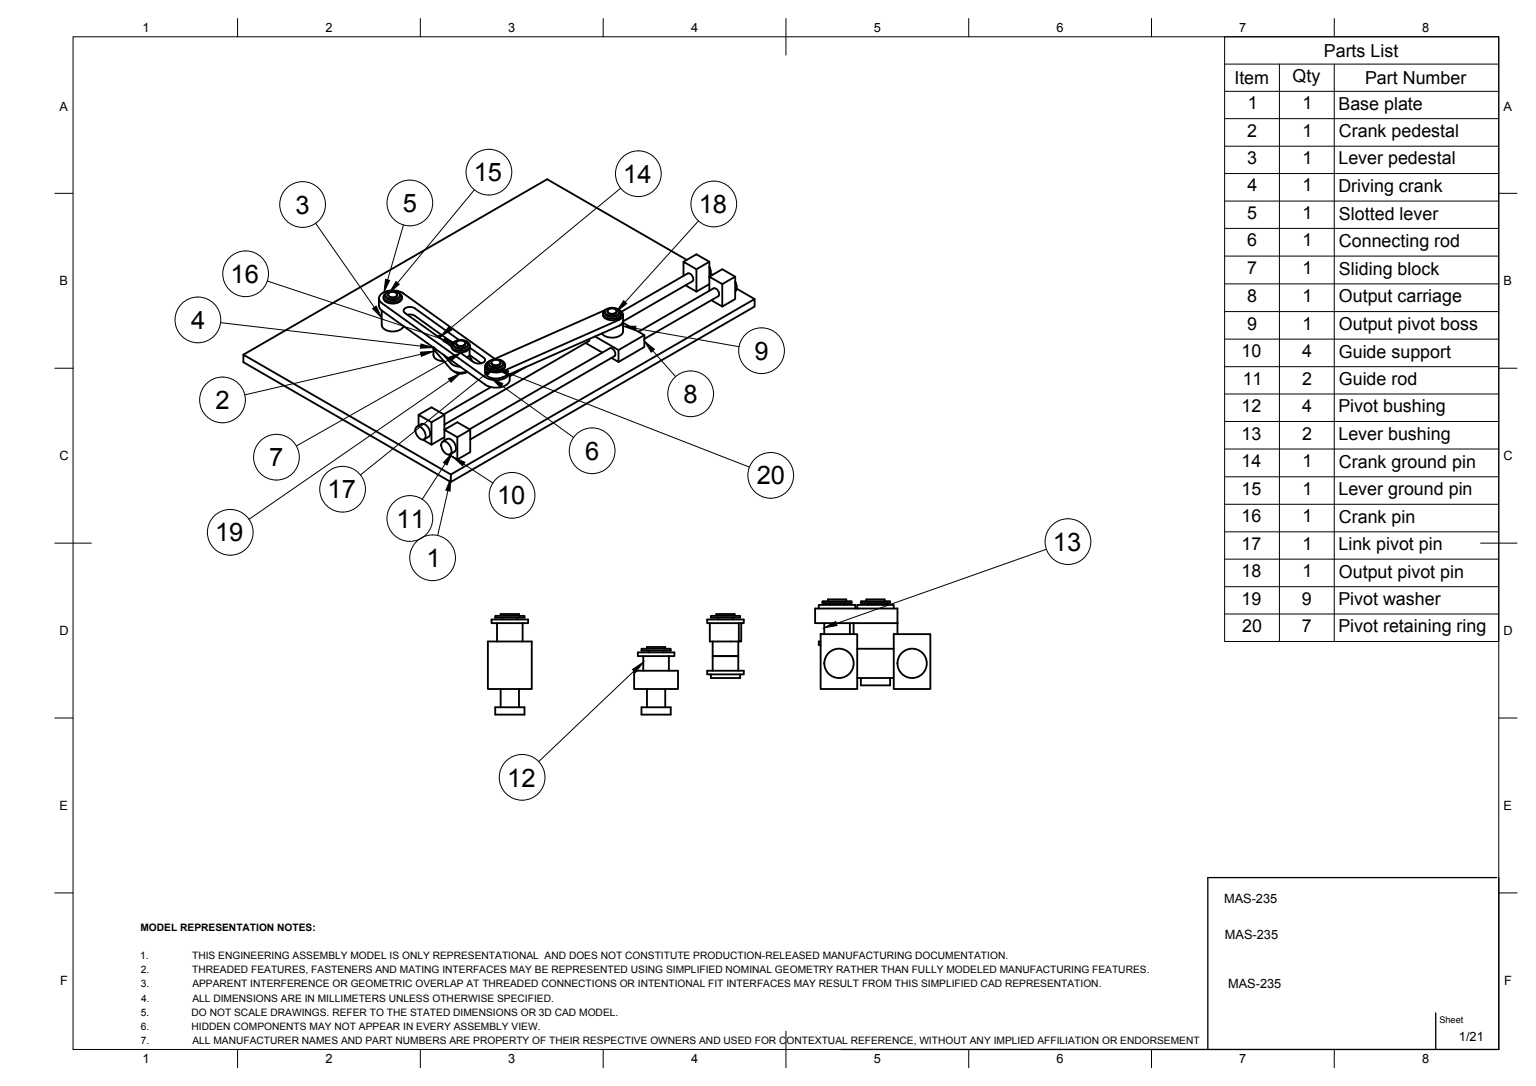
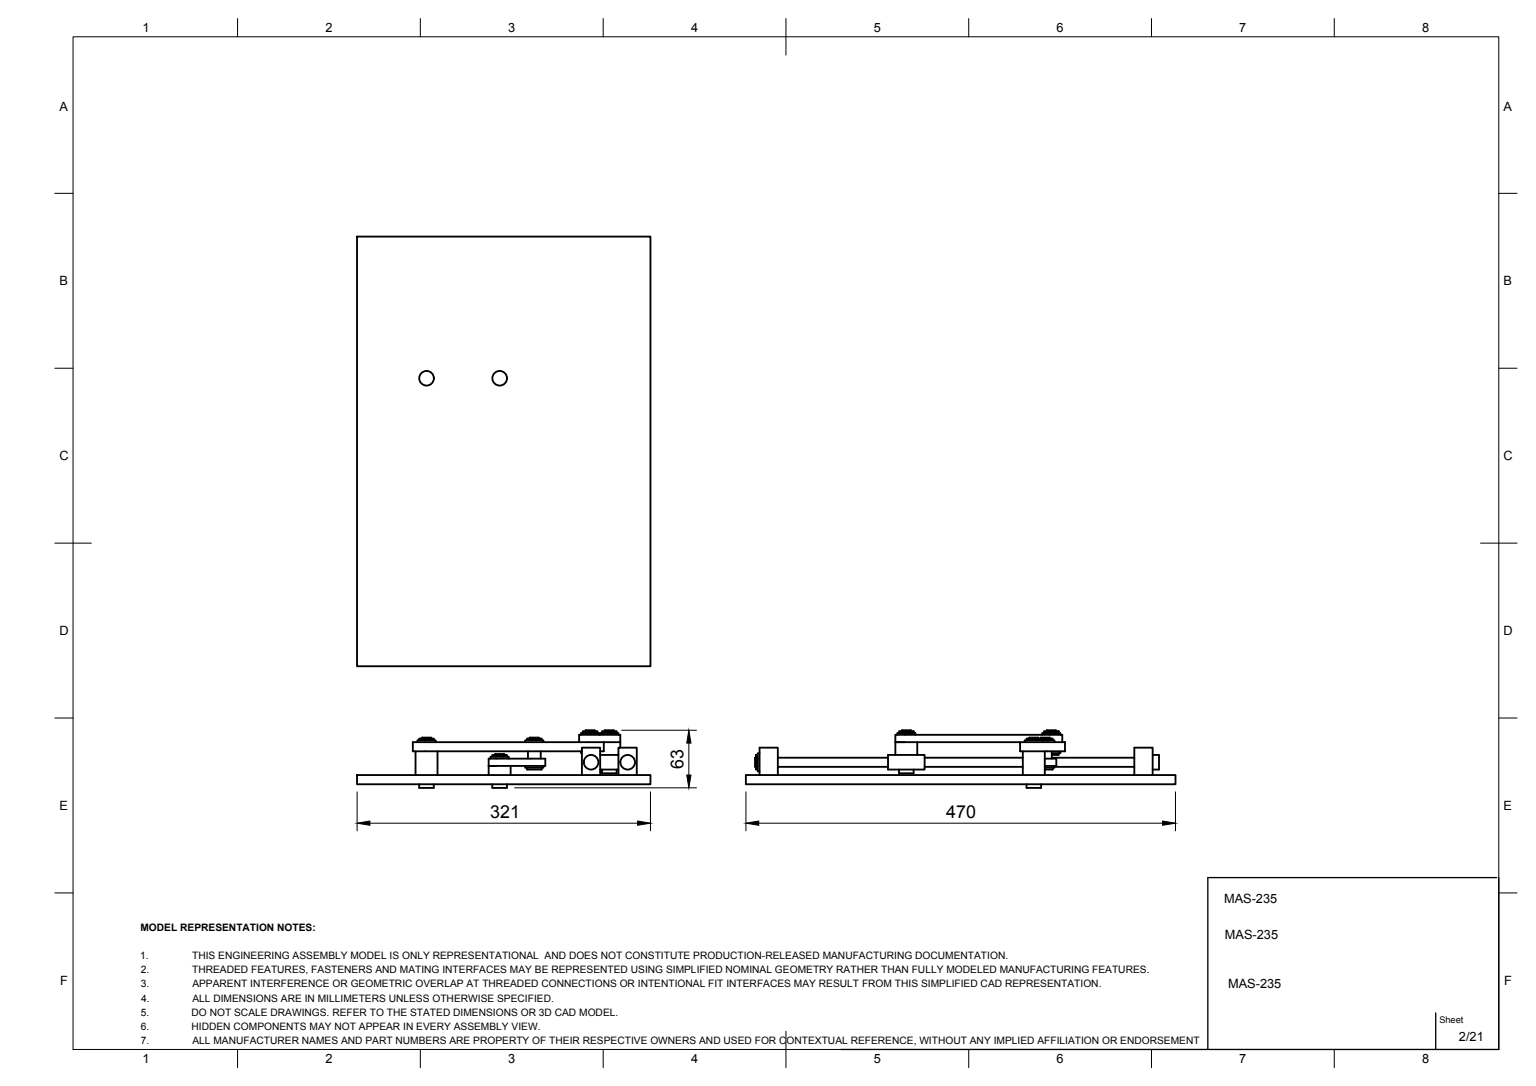
ISO-10303-21;
HEADER;
/* Generated by software containing ST-Developer
 * from STEP Tools, Inc. (www.steptools.com) 
 */

FILE_DESCRIPTION(
/* description */ ('Independent Whitworth quick-return mechanism. Crank radius40, ground-
center spacing80, lever180, connecting rod160, output guide X200. Nomi
nal stroke180 and long/short phase ratio2. Retained guide rods, replac
eable bearing sleeves and captured sliding shoe. No load or production
 rating assigned.'),
/* implementation_level */ '2;1');

FILE_NAME(
/* name */ 'MAS-235.step',
/* time_stamp */ '2026-11-09T18:22:56-08:00',
/* author */ (''),
/* organization */ (''),
/* preprocessor_version */ 'ST-DEVELOPER v20.2',
/* originating_system */ 'Autodesk Translation Framework v15.17.0.0',
/* authorisation */ '');

FILE_SCHEMA (('AUTOMOTIVE_DESIGN { 1 0 10303 214 3 1 1 }'));
ENDSEC;

DATA;
#10=MECHANICAL_DESIGN_GEOMETRIC_PRESENTATION_REPRESENTATION('',(#219,#220,
#221,#222,#223,#224,#225,#226,#227,#228,#229,#230,#231,#232,#233,#234,#235,
#236,#237,#238),#4388);
#11=ITEM_DEFINED_TRANSFORMATION($,$,#2566,#2855);
#12=ITEM_DEFINED_TRANSFORMATION($,$,#2579,#2856);
#13=ITEM_DEFINED_TRANSFORMATION($,$,#2588,#2857);
#14=ITEM_DEFINED_TRANSFORMATION($,$,#2597,#2858);
#15=ITEM_DEFINED_TRANSFORMATION($,$,#2614,#2859);
#16=ITEM_DEFINED_TRANSFORMATION($,$,#2639,#2860);
#17=ITEM_DEFINED_TRANSFORMATION($,$,#2656,#2861);
#18=ITEM_DEFINED_TRANSFORMATION($,$,#2666,#2862);
#19=ITEM_DEFINED_TRANSFORMATION($,$,#2682,#2863);
#20=ITEM_DEFINED_TRANSFORMATION($,$,#2691,#2864);
#21=ITEM_DEFINED_TRANSFORMATION($,$,#2701,#2865);
#22=ITEM_DEFINED_TRANSFORMATION($,$,#2817,#2866);
#23=ITEM_DEFINED_TRANSFORMATION($,$,#2691,#2867);
#24=ITEM_DEFINED_TRANSFORMATION($,$,#2691,#2868);
#25=ITEM_DEFINED_TRANSFORMATION($,$,#2691,#2869);
#26=ITEM_DEFINED_TRANSFORMATION($,$,#2701,#2870);
#27=ITEM_DEFINED_TRANSFORMATION($,$,#2826,#2871);
#28=ITEM_DEFINED_TRANSFORMATION($,$,#2719,#2872);
#29=ITEM_DEFINED_TRANSFORMATION($,$,#2737,#2873);
#30=ITEM_DEFINED_TRANSFORMATION($,$,#2755,#2874);
#31=ITEM_DEFINED_TRANSFORMATION($,$,#2781,#2875);
#32=ITEM_DEFINED_TRANSFORMATION($,$,#2799,#2876);
#33=ITEM_DEFINED_TRANSFORMATION($,$,#2835,#2877);
#34=ITEM_DEFINED_TRANSFORMATION($,$,#2817,#2878);
#35=ITEM_DEFINED_TRANSFORMATION($,$,#2817,#2879);
#36=ITEM_DEFINED_TRANSFORMATION($,$,#2817,#2880);
#37=ITEM_DEFINED_TRANSFORMATION($,$,#2826,#2881);
#38=ITEM_DEFINED_TRANSFORMATION($,$,#2844,#2882);
#39=ITEM_DEFINED_TRANSFORMATION($,$,#2835,#2883);
#40=ITEM_DEFINED_TRANSFORMATION($,$,#2835,#2884);
#41=ITEM_DEFINED_TRANSFORMATION($,$,#2835,#2885);
#42=ITEM_DEFINED_TRANSFORMATION($,$,#2835,#2886);
#43=ITEM_DEFINED_TRANSFORMATION($,$,#2835,#2887);
#44=ITEM_DEFINED_TRANSFORMATION($,$,#2835,#2888);
#45=ITEM_DEFINED_TRANSFORMATION($,$,#2835,#2889);
#46=ITEM_DEFINED_TRANSFORMATION($,$,#2835,#2890);
#47=ITEM_DEFINED_TRANSFORMATION($,$,#2844,#2891);
#48=ITEM_DEFINED_TRANSFORMATION($,$,#2844,#2892);
#49=ITEM_DEFINED_TRANSFORMATION($,$,#2844,#2893);
#50=ITEM_DEFINED_TRANSFORMATION($,$,#2844,#2894);
#51=ITEM_DEFINED_TRANSFORMATION($,$,#2844,#2895);
#52=ITEM_DEFINED_TRANSFORMATION($,$,#2844,#2896);
#53=(
REPRESENTATION_RELATIONSHIP($,$,#4478,#4477)
REPRESENTATION_RELATIONSHIP_WITH_TRANSFORMATION(#11)
SHAPE_REPRESENTATION_RELATIONSHIP()
);
#54=(
REPRESENTATION_RELATIONSHIP($,$,#4479,#4477)
REPRESENTATION_RELATIONSHIP_WITH_TRANSFORMATION(#12)
SHAPE_REPRESENTATION_RELATIONSHIP()
);
#55=(
REPRESENTATION_RELATIONSHIP($,$,#4480,#4477)
REPRESENTATION_RELATIONSHIP_WITH_TRANSFORMATION(#13)
SHAPE_REPRESENTATION_RELATIONSHIP()
);
#56=(
REPRESENTATION_RELATIONSHIP($,$,#4481,#4477)
REPRESENTATION_RELATIONSHIP_WITH_TRANSFORMATION(#14)
SHAPE_REPRESENTATION_RELATIONSHIP()
);
#57=(
REPRESENTATION_RELATIONSHIP($,$,#4482,#4477)
REPRESENTATION_RELATIONSHIP_WITH_TRANSFORMATION(#15)
SHAPE_REPRESENTATION_RELATIONSHIP()
);
#58=(
REPRESENTATION_RELATIONSHIP($,$,#4483,#4477)
REPRESENTATION_RELATIONSHIP_WITH_TRANSFORMATION(#16)
SHAPE_REPRESENTATION_RELATIONSHIP()
);
#59=(
REPRESENTATION_RELATIONSHIP($,$,#4484,#4477)
REPRESENTATION_RELATIONSHIP_WITH_TRANSFORMATION(#17)
SHAPE_REPRESENTATION_RELATIONSHIP()
);
#60=(
REPRESENTATION_RELATIONSHIP($,$,#4485,#4477)
REPRESENTATION_RELATIONSHIP_WITH_TRANSFORMATION(#18)
SHAPE_REPRESENTATION_RELATIONSHIP()
);
#61=(
REPRESENTATION_RELATIONSHIP($,$,#4486,#4477)
REPRESENTATION_RELATIONSHIP_WITH_TRANSFORMATION(#19)
SHAPE_REPRESENTATION_RELATIONSHIP()
);
#62=(
REPRESENTATION_RELATIONSHIP($,$,#4487,#4477)
REPRESENTATION_RELATIONSHIP_WITH_TRANSFORMATION(#20)
SHAPE_REPRESENTATION_RELATIONSHIP()
);
#63=(
REPRESENTATION_RELATIONSHIP($,$,#4488,#4477)
REPRESENTATION_RELATIONSHIP_WITH_TRANSFORMATION(#21)
SHAPE_REPRESENTATION_RELATIONSHIP()
);
#64=(
REPRESENTATION_RELATIONSHIP($,$,#4494,#4477)
REPRESENTATION_RELATIONSHIP_WITH_TRANSFORMATION(#22)
SHAPE_REPRESENTATION_RELATIONSHIP()
);
#65=(
REPRESENTATION_RELATIONSHIP($,$,#4487,#4477)
REPRESENTATION_RELATIONSHIP_WITH_TRANSFORMATION(#23)
SHAPE_REPRESENTATION_RELATIONSHIP()
);
#66=(
REPRESENTATION_RELATIONSHIP($,$,#4487,#4477)
REPRESENTATION_RELATIONSHIP_WITH_TRANSFORMATION(#24)
SHAPE_REPRESENTATION_RELATIONSHIP()
);
#67=(
REPRESENTATION_RELATIONSHIP($,$,#4487,#4477)
REPRESENTATION_RELATIONSHIP_WITH_TRANSFORMATION(#25)
SHAPE_REPRESENTATION_RELATIONSHIP()
);
#68=(
REPRESENTATION_RELATIONSHIP($,$,#4488,#4477)
REPRESENTATION_RELATIONSHIP_WITH_TRANSFORMATION(#26)
SHAPE_REPRESENTATION_RELATIONSHIP()
);
#69=(
REPRESENTATION_RELATIONSHIP($,$,#4495,#4477)
REPRESENTATION_RELATIONSHIP_WITH_TRANSFORMATION(#27)
SHAPE_REPRESENTATION_RELATIONSHIP()
);
#70=(
REPRESENTATION_RELATIONSHIP($,$,#4489,#4477)
REPRESENTATION_RELATIONSHIP_WITH_TRANSFORMATION(#28)
SHAPE_REPRESENTATION_RELATIONSHIP()
);
#71=(
REPRESENTATION_RELATIONSHIP($,$,#4490,#4477)
REPRESENTATION_RELATIONSHIP_WITH_TRANSFORMATION(#29)
SHAPE_REPRESENTATION_RELATIONSHIP()
);
#72=(
REPRESENTATION_RELATIONSHIP($,$,#4491,#4477)
REPRESENTATION_RELATIONSHIP_WITH_TRANSFORMATION(#30)
SHAPE_REPRESENTATION_RELATIONSHIP()
);
#73=(
REPRESENTATION_RELATIONSHIP($,$,#4492,#4477)
REPRESENTATION_RELATIONSHIP_WITH_TRANSFORMATION(#31)
SHAPE_REPRESENTATION_RELATIONSHIP()
);
#74=(
REPRESENTATION_RELATIONSHIP($,$,#4493,#4477)
REPRESENTATION_RELATIONSHIP_WITH_TRANSFORMATION(#32)
SHAPE_REPRESENTATION_RELATIONSHIP()
);
#75=(
REPRESENTATION_RELATIONSHIP($,$,#4496,#4477)
REPRESENTATION_RELATIONSHIP_WITH_TRANSFORMATION(#33)
SHAPE_REPRESENTATION_RELATIONSHIP()
);
#76=(
REPRESENTATION_RELATIONSHIP($,$,#4494,#4477)
REPRESENTATION_RELATIONSHIP_WITH_TRANSFORMATION(#34)
SHAPE_REPRESENTATION_RELATIONSHIP()
);
#77=(
REPRESENTATION_RELATIONSHIP($,$,#4494,#4477)
REPRESENTATION_RELATIONSHIP_WITH_TRANSFORMATION(#35)
SHAPE_REPRESENTATION_RELATIONSHIP()
);
#78=(
REPRESENTATION_RELATIONSHIP($,$,#4494,#4477)
REPRESENTATION_RELATIONSHIP_WITH_TRANSFORMATION(#36)
SHAPE_REPRESENTATION_RELATIONSHIP()
);
#79=(
REPRESENTATION_RELATIONSHIP($,$,#4495,#4477)
REPRESENTATION_RELATIONSHIP_WITH_TRANSFORMATION(#37)
SHAPE_REPRESENTATION_RELATIONSHIP()
);
#80=(
REPRESENTATION_RELATIONSHIP($,$,#4497,#4477)
REPRESENTATION_RELATIONSHIP_WITH_TRANSFORMATION(#38)
SHAPE_REPRESENTATION_RELATIONSHIP()
);
#81=(
REPRESENTATION_RELATIONSHIP($,$,#4496,#4477)
REPRESENTATION_RELATIONSHIP_WITH_TRANSFORMATION(#39)
SHAPE_REPRESENTATION_RELATIONSHIP()
);
#82=(
REPRESENTATION_RELATIONSHIP($,$,#4496,#4477)
REPRESENTATION_RELATIONSHIP_WITH_TRANSFORMATION(#40)
SHAPE_REPRESENTATION_RELATIONSHIP()
);
#83=(
REPRESENTATION_RELATIONSHIP($,$,#4496,#4477)
REPRESENTATION_RELATIONSHIP_WITH_TRANSFORMATION(#41)
SHAPE_REPRESENTATION_RELATIONSHIP()
);
#84=(
REPRESENTATION_RELATIONSHIP($,$,#4496,#4477)
REPRESENTATION_RELATIONSHIP_WITH_TRANSFORMATION(#42)
SHAPE_REPRESENTATION_RELATIONSHIP()
);
#85=(
REPRESENTATION_RELATIONSHIP($,$,#4496,#4477)
REPRESENTATION_RELATIONSHIP_WITH_TRANSFORMATION(#43)
SHAPE_REPRESENTATION_RELATIONSHIP()
);
#86=(
REPRESENTATION_RELATIONSHIP($,$,#4496,#4477)
REPRESENTATION_RELATIONSHIP_WITH_TRANSFORMATION(#44)
SHAPE_REPRESENTATION_RELATIONSHIP()
);
#87=(
REPRESENTATION_RELATIONSHIP($,$,#4496,#4477)
REPRESENTATION_RELATIONSHIP_WITH_TRANSFORMATION(#45)
SHAPE_REPRESENTATION_RELATIONSHIP()
);
#88=(
REPRESENTATION_RELATIONSHIP($,$,#4496,#4477)
REPRESENTATION_RELATIONSHIP_WITH_TRANSFORMATION(#46)
SHAPE_REPRESENTATION_RELATIONSHIP()
);
#89=(
REPRESENTATION_RELATIONSHIP($,$,#4497,#4477)
REPRESENTATION_RELATIONSHIP_WITH_TRANSFORMATION(#47)
SHAPE_REPRESENTATION_RELATIONSHIP()
);
#90=(
REPRESENTATION_RELATIONSHIP($,$,#4497,#4477)
REPRESENTATION_RELATIONSHIP_WITH_TRANSFORMATION(#48)
SHAPE_REPRESENTATION_RELATIONSHIP()
);
#91=(
REPRESENTATION_RELATIONSHIP($,$,#4497,#4477)
REPRESENTATION_RELATIONSHIP_WITH_TRANSFORMATION(#49)
SHAPE_REPRESENTATION_RELATIONSHIP()
);
#92=(
REPRESENTATION_RELATIONSHIP($,$,#4497,#4477)
REPRESENTATION_RELATIONSHIP_WITH_TRANSFORMATION(#50)
SHAPE_REPRESENTATION_RELATIONSHIP()
);
#93=(
REPRESENTATION_RELATIONSHIP($,$,#4497,#4477)
REPRESENTATION_RELATIONSHIP_WITH_TRANSFORMATION(#51)
SHAPE_REPRESENTATION_RELATIONSHIP()
);
#94=(
REPRESENTATION_RELATIONSHIP($,$,#4497,#4477)
REPRESENTATION_RELATIONSHIP_WITH_TRANSFORMATION(#52)
SHAPE_REPRESENTATION_RELATIONSHIP()
);
#95=CONTEXT_DEPENDENT_SHAPE_REPRESENTATION(#53,#4435);
#96=CONTEXT_DEPENDENT_SHAPE_REPRESENTATION(#54,#4436);
#97=CONTEXT_DEPENDENT_SHAPE_REPRESENTATION(#55,#4437);
#98=CONTEXT_DEPENDENT_SHAPE_REPRESENTATION(#56,#4438);
#99=CONTEXT_DEPENDENT_SHAPE_REPRESENTATION(#57,#4439);
#100=CONTEXT_DEPENDENT_SHAPE_REPRESENTATION(#58,#4440);
#101=CONTEXT_DEPENDENT_SHAPE_REPRESENTATION(#59,#4441);
#102=CONTEXT_DEPENDENT_SHAPE_REPRESENTATION(#60,#4442);
#103=CONTEXT_DEPENDENT_SHAPE_REPRESENTATION(#61,#4443);
#104=CONTEXT_DEPENDENT_SHAPE_REPRESENTATION(#62,#4444);
#105=CONTEXT_DEPENDENT_SHAPE_REPRESENTATION(#63,#4445);
#106=CONTEXT_DEPENDENT_SHAPE_REPRESENTATION(#64,#4446);
#107=CONTEXT_DEPENDENT_SHAPE_REPRESENTATION(#65,#4447);
#108=CONTEXT_DEPENDENT_SHAPE_REPRESENTATION(#66,#4448);
#109=CONTEXT_DEPENDENT_SHAPE_REPRESENTATION(#67,#4449);
#110=CONTEXT_DEPENDENT_SHAPE_REPRESENTATION(#68,#4450);
#111=CONTEXT_DEPENDENT_SHAPE_REPRESENTATION(#69,#4451);
#112=CONTEXT_DEPENDENT_SHAPE_REPRESENTATION(#70,#4452);
#113=CONTEXT_DEPENDENT_SHAPE_REPRESENTATION(#71,#4453);
#114=CONTEXT_DEPENDENT_SHAPE_REPRESENTATION(#72,#4454);
#115=CONTEXT_DEPENDENT_SHAPE_REPRESENTATION(#73,#4455);
#116=CONTEXT_DEPENDENT_SHAPE_REPRESENTATION(#74,#4456);
#117=CONTEXT_DEPENDENT_SHAPE_REPRESENTATION(#75,#4457);
#118=CONTEXT_DEPENDENT_SHAPE_REPRESENTATION(#76,#4458);
#119=CONTEXT_DEPENDENT_SHAPE_REPRESENTATION(#77,#4459);
#120=CONTEXT_DEPENDENT_SHAPE_REPRESENTATION(#78,#4460);
#121=CONTEXT_DEPENDENT_SHAPE_REPRESENTATION(#79,#4461);
#122=CONTEXT_DEPENDENT_SHAPE_REPRESENTATION(#80,#4462);
#123=CONTEXT_DEPENDENT_SHAPE_REPRESENTATION(#81,#4463);
#124=CONTEXT_DEPENDENT_SHAPE_REPRESENTATION(#82,#4464);
#125=CONTEXT_DEPENDENT_SHAPE_REPRESENTATION(#83,#4465);
#126=CONTEXT_DEPENDENT_SHAPE_REPRESENTATION(#84,#4466);
#127=CONTEXT_DEPENDENT_SHAPE_REPRESENTATION(#85,#4467);
#128=CONTEXT_DEPENDENT_SHAPE_REPRESENTATION(#86,#4468);
#129=CONTEXT_DEPENDENT_SHAPE_REPRESENTATION(#87,#4469);
#130=CONTEXT_DEPENDENT_SHAPE_REPRESENTATION(#88,#4470);
#131=CONTEXT_DEPENDENT_SHAPE_REPRESENTATION(#89,#4471);
#132=CONTEXT_DEPENDENT_SHAPE_REPRESENTATION(#90,#4472);
#133=CONTEXT_DEPENDENT_SHAPE_REPRESENTATION(#91,#4473);
#134=CONTEXT_DEPENDENT_SHAPE_REPRESENTATION(#92,#4474);
#135=CONTEXT_DEPENDENT_SHAPE_REPRESENTATION(#93,#4475);
#136=CONTEXT_DEPENDENT_SHAPE_REPRESENTATION(#94,#4476);
#137=NEXT_ASSEMBLY_USAGE_OCCURRENCE('Base plate:1','Base plate:1',
'Base plate:1',#4499,#4500,'Base plate:1');
#138=NEXT_ASSEMBLY_USAGE_OCCURRENCE('Crank pedestal:1',
'Crank pedestal:1','Crank pedestal:1',#4499,#4501,'Crank pedestal:1');
#139=NEXT_ASSEMBLY_USAGE_OCCURRENCE('Lever pedestal:1',
'Lever pedestal:1','Lever pedestal:1',#4499,#4502,'Lever pedestal:1');
#140=NEXT_ASSEMBLY_USAGE_OCCURRENCE('Driving crank:1','Driving crank:1',
'Driving crank:1',#4499,#4503,'Driving crank:1');
#141=NEXT_ASSEMBLY_USAGE_OCCURRENCE('Slotted lever:1','Slotted lever:1',
'Slotted lever:1',#4499,#4504,'Slotted lever:1');
#142=NEXT_ASSEMBLY_USAGE_OCCURRENCE('Connecting rod:1',
'Connecting rod:1','Connecting rod:1',#4499,#4505,'Connecting rod:1');
#143=NEXT_ASSEMBLY_USAGE_OCCURRENCE('Sliding block:1','Sliding block:1',
'Sliding block:1',#4499,#4506,'Sliding block:1');
#144=NEXT_ASSEMBLY_USAGE_OCCURRENCE('Output carriage:1',
'Output carriage:1','Output carriage:1',#4499,#4507,'Output carriage:1');
#145=NEXT_ASSEMBLY_USAGE_OCCURRENCE('Output pivot boss:1',
'Output pivot boss:1','Output pivot boss:1',#4499,#4508,
'Output pivot boss:1');
#146=NEXT_ASSEMBLY_USAGE_OCCURRENCE('Guide support:1','Guide support:1',
'Guide support:1',#4499,#4509,'Guide support:1');
#147=NEXT_ASSEMBLY_USAGE_OCCURRENCE('Guide rod:1','Guide rod:1',
'Guide rod:1',#4499,#4510,'Guide rod:1');
#148=NEXT_ASSEMBLY_USAGE_OCCURRENCE('Pivot bushing:1','Pivot bushing:1',
'Pivot bushing:1',#4499,#4516,'Pivot bushing:1');
#149=NEXT_ASSEMBLY_USAGE_OCCURRENCE('Guide support:2','Guide support:2',
'Guide support:2',#4499,#4509,'Guide support:2');
#150=NEXT_ASSEMBLY_USAGE_OCCURRENCE('Guide support:3','Guide support:3',
'Guide support:3',#4499,#4509,'Guide support:3');
#151=NEXT_ASSEMBLY_USAGE_OCCURRENCE('Guide support:4','Guide support:4',
'Guide support:4',#4499,#4509,'Guide support:4');
#152=NEXT_ASSEMBLY_USAGE_OCCURRENCE('Guide rod:2','Guide rod:2',
'Guide rod:2',#4499,#4510,'Guide rod:2');
#153=NEXT_ASSEMBLY_USAGE_OCCURRENCE('Lever bushing:1','Lever bushing:1',
'Lever bushing:1',#4499,#4517,'Lever bushing:1');
#154=NEXT_ASSEMBLY_USAGE_OCCURRENCE('Crank ground pin:1',
'Crank ground pin:1','Crank ground pin:1',#4499,#4511,
'Crank ground pin:1');
#155=NEXT_ASSEMBLY_USAGE_OCCURRENCE('Lever ground pin:1',
'Lever ground pin:1','Lever ground pin:1',#4499,#4512,
'Lever ground pin:1');
#156=NEXT_ASSEMBLY_USAGE_OCCURRENCE('Crank pin:1','Crank pin:1',
'Crank pin:1',#4499,#4513,'Crank pin:1');
#157=NEXT_ASSEMBLY_USAGE_OCCURRENCE('Link pivot pin:1',
'Link pivot pin:1','Link pivot pin:1',#4499,#4514,'Link pivot pin:1');
#158=NEXT_ASSEMBLY_USAGE_OCCURRENCE('Output pivot pin:1',
'Output pivot pin:1','Output pivot pin:1',#4499,#4515,
'Output pivot pin:1');
#159=NEXT_ASSEMBLY_USAGE_OCCURRENCE('Pivot washer:1','Pivot washer:1',
'Pivot washer:1',#4499,#4518,'Pivot washer:1');
#160=NEXT_ASSEMBLY_USAGE_OCCURRENCE('Pivot bushing:2','Pivot bushing:2',
'Pivot bushing:2',#4499,#4516,'Pivot bushing:2');
#161=NEXT_ASSEMBLY_USAGE_OCCURRENCE('Pivot bushing:3','Pivot bushing:3',
'Pivot bushing:3',#4499,#4516,'Pivot bushing:3');
#162=NEXT_ASSEMBLY_USAGE_OCCURRENCE('Pivot bushing:4','Pivot bushing:4',
'Pivot bushing:4',#4499,#4516,'Pivot bushing:4');
#163=NEXT_ASSEMBLY_USAGE_OCCURRENCE('Lever bushing:2','Lever bushing:2',
'Lever bushing:2',#4499,#4517,'Lever bushing:2');
#164=NEXT_ASSEMBLY_USAGE_OCCURRENCE('Pivot retaining ring:1',
'Pivot retaining ring:1','Pivot retaining ring:1',#4499,#4519,
'Pivot retaining ring:1');
#165=NEXT_ASSEMBLY_USAGE_OCCURRENCE('Pivot washer:2','Pivot washer:2',
'Pivot washer:2',#4499,#4518,'Pivot washer:2');
#166=NEXT_ASSEMBLY_USAGE_OCCURRENCE('Pivot washer:3','Pivot washer:3',
'Pivot washer:3',#4499,#4518,'Pivot washer:3');
#167=NEXT_ASSEMBLY_USAGE_OCCURRENCE('Pivot washer:4','Pivot washer:4',
'Pivot washer:4',#4499,#4518,'Pivot washer:4');
#168=NEXT_ASSEMBLY_USAGE_OCCURRENCE('Pivot washer:5','Pivot washer:5',
'Pivot washer:5',#4499,#4518,'Pivot washer:5');
#169=NEXT_ASSEMBLY_USAGE_OCCURRENCE('Pivot washer:6','Pivot washer:6',
'Pivot washer:6',#4499,#4518,'Pivot washer:6');
#170=NEXT_ASSEMBLY_USAGE_OCCURRENCE('Pivot washer:7','Pivot washer:7',
'Pivot washer:7',#4499,#4518,'Pivot washer:7');
#171=NEXT_ASSEMBLY_USAGE_OCCURRENCE('Pivot washer:8','Pivot washer:8',
'Pivot washer:8',#4499,#4518,'Pivot washer:8');
#172=NEXT_ASSEMBLY_USAGE_OCCURRENCE('Pivot washer:9','Pivot washer:9',
'Pivot washer:9',#4499,#4518,'Pivot washer:9');
#173=NEXT_ASSEMBLY_USAGE_OCCURRENCE('Pivot retaining ring:2',
'Pivot retaining ring:2','Pivot retaining ring:2',#4499,#4519,
'Pivot retaining ring:2');
#174=NEXT_ASSEMBLY_USAGE_OCCURRENCE('Pivot retaining ring:3',
'Pivot retaining ring:3','Pivot retaining ring:3',#4499,#4519,
'Pivot retaining ring:3');
#175=NEXT_ASSEMBLY_USAGE_OCCURRENCE('Pivot retaining ring:4',
'Pivot retaining ring:4','Pivot retaining ring:4',#4499,#4519,
'Pivot retaining ring:4');
#176=NEXT_ASSEMBLY_USAGE_OCCURRENCE('Pivot retaining ring:5',
'Pivot retaining ring:5','Pivot retaining ring:5',#4499,#4519,
'Pivot retaining ring:5');
#177=NEXT_ASSEMBLY_USAGE_OCCURRENCE('Pivot retaining ring:6',
'Pivot retaining ring:6','Pivot retaining ring:6',#4499,#4519,
'Pivot retaining ring:6');
#178=NEXT_ASSEMBLY_USAGE_OCCURRENCE('Pivot retaining ring:7',
'Pivot retaining ring:7','Pivot retaining ring:7',#4499,#4519,
'Pivot retaining ring:7');
#179=SHAPE_REPRESENTATION_RELATIONSHIP('SRR','None',#4478,#199);
#180=SHAPE_REPRESENTATION_RELATIONSHIP('SRR','None',#4479,#200);
#181=SHAPE_REPRESENTATION_RELATIONSHIP('SRR','None',#4480,#201);
#182=SHAPE_REPRESENTATION_RELATIONSHIP('SRR','None',#4481,#202);
#183=SHAPE_REPRESENTATION_RELATIONSHIP('SRR','None',#4482,#203);
#184=SHAPE_REPRESENTATION_RELATIONSHIP('SRR','None',#4483,#204);
#185=SHAPE_REPRESENTATION_RELATIONSHIP('SRR','None',#4484,#205);
#186=SHAPE_REPRESENTATION_RELATIONSHIP('SRR','None',#4485,#206);
#187=SHAPE_REPRESENTATION_RELATIONSHIP('SRR','None',#4486,#207);
#188=SHAPE_REPRESENTATION_RELATIONSHIP('SRR','None',#4487,#208);
#189=SHAPE_REPRESENTATION_RELATIONSHIP('SRR','None',#4488,#209);
#190=SHAPE_REPRESENTATION_RELATIONSHIP('SRR','None',#4489,#210);
#191=SHAPE_REPRESENTATION_RELATIONSHIP('SRR','None',#4490,#211);
#192=SHAPE_REPRESENTATION_RELATIONSHIP('SRR','None',#4491,#212);
#193=SHAPE_REPRESENTATION_RELATIONSHIP('SRR','None',#4492,#213);
#194=SHAPE_REPRESENTATION_RELATIONSHIP('SRR','None',#4493,#214);
#195=SHAPE_REPRESENTATION_RELATIONSHIP('SRR','None',#4494,#215);
#196=SHAPE_REPRESENTATION_RELATIONSHIP('SRR','None',#4495,#216);
#197=SHAPE_REPRESENTATION_RELATIONSHIP('SRR','None',#4496,#217);
#198=SHAPE_REPRESENTATION_RELATIONSHIP('SRR','None',#4497,#218);
#199=ADVANCED_BREP_SHAPE_REPRESENTATION('',(#239),#4368);
#200=ADVANCED_BREP_SHAPE_REPRESENTATION('',(#240),#4369);
#201=ADVANCED_BREP_SHAPE_REPRESENTATION('',(#241),#4370);
#202=ADVANCED_BREP_SHAPE_REPRESENTATION('',(#242),#4371);
#203=ADVANCED_BREP_SHAPE_REPRESENTATION('',(#243),#4372);
#204=ADVANCED_BREP_SHAPE_REPRESENTATION('',(#244),#4373);
#205=ADVANCED_BREP_SHAPE_REPRESENTATION('',(#245),#4374);
#206=ADVANCED_BREP_SHAPE_REPRESENTATION('',(#246),#4375);
#207=ADVANCED_BREP_SHAPE_REPRESENTATION('',(#247),#4376);
#208=ADVANCED_BREP_SHAPE_REPRESENTATION('',(#248),#4377);
#209=ADVANCED_BREP_SHAPE_REPRESENTATION('',(#249),#4378);
#210=ADVANCED_BREP_SHAPE_REPRESENTATION('',(#250),#4379);
#211=ADVANCED_BREP_SHAPE_REPRESENTATION('',(#251),#4380);
#212=ADVANCED_BREP_SHAPE_REPRESENTATION('',(#252),#4381);
#213=ADVANCED_BREP_SHAPE_REPRESENTATION('',(#253),#4382);
#214=ADVANCED_BREP_SHAPE_REPRESENTATION('',(#254),#4383);
#215=ADVANCED_BREP_SHAPE_REPRESENTATION('',(#255),#4384);
#216=ADVANCED_BREP_SHAPE_REPRESENTATION('',(#256),#4385);
#217=ADVANCED_BREP_SHAPE_REPRESENTATION('',(#257),#4386);
#218=ADVANCED_BREP_SHAPE_REPRESENTATION('',(#258),#4387);
#219=STYLED_ITEM('',(#4587),#239);
#220=STYLED_ITEM('',(#4588),#240);
#221=STYLED_ITEM('',(#4588),#241);
#222=STYLED_ITEM('',(#4589),#242);
#223=STYLED_ITEM('',(#4590),#243);
#224=STYLED_ITEM('',(#4591),#244);
#225=STYLED_ITEM('',(#4592),#245);
#226=STYLED_ITEM('',(#4593),#246);
#227=STYLED_ITEM('',(#4594),#247);
#228=STYLED_ITEM('',(#4588),#248);
#229=STYLED_ITEM('',(#4595),#249);
#230=STYLED_ITEM('',(#4595),#250);
#231=STYLED_ITEM('',(#4595),#251);
#232=STYLED_ITEM('',(#4595),#252);
#233=STYLED_ITEM('',(#4595),#253);
#234=STYLED_ITEM('',(#4595),#254);
#235=STYLED_ITEM('',(#4596),#255);
#236=STYLED_ITEM('',(#4597),#256);
#237=STYLED_ITEM('',(#4598),#257);
#238=STYLED_ITEM('',(#4599),#258);
#239=MANIFOLD_SOLID_BREP('Body1',#2324);
#240=MANIFOLD_SOLID_BREP('Body1',#2325);
#241=MANIFOLD_SOLID_BREP('Body1',#2326);
#242=MANIFOLD_SOLID_BREP('Body1',#2327);
#243=MANIFOLD_SOLID_BREP('Body1',#2328);
#244=MANIFOLD_SOLID_BREP('Body1',#2329);
#245=MANIFOLD_SOLID_BREP('Body1',#2330);
#246=MANIFOLD_SOLID_BREP('Body1',#2331);
#247=MANIFOLD_SOLID_BREP('Body1',#2332);
#248=MANIFOLD_SOLID_BREP('Body1',#2333);
#249=MANIFOLD_SOLID_BREP('Body1',#2334);
#250=MANIFOLD_SOLID_BREP('Body1',#2335);
#251=MANIFOLD_SOLID_BREP('Body1',#2336);
#252=MANIFOLD_SOLID_BREP('Body1',#2337);
#253=MANIFOLD_SOLID_BREP('Body1',#2338);
#254=MANIFOLD_SOLID_BREP('Body1',#2339);
#255=MANIFOLD_SOLID_BREP('Body1',#2340);
#256=MANIFOLD_SOLID_BREP('Body1',#2341);
#257=MANIFOLD_SOLID_BREP('Body1',#2342);
#258=MANIFOLD_SOLID_BREP('Body1',#2343);
#259=FACE_BOUND('',#559,.T.);
#260=FACE_BOUND('',#560,.T.);
#261=FACE_BOUND('',#562,.T.);
#262=FACE_BOUND('',#563,.T.);
#263=FACE_BOUND('',#567,.T.);
#264=FACE_BOUND('',#569,.T.);
#265=FACE_BOUND('',#573,.T.);
#266=FACE_BOUND('',#575,.T.);
#267=FACE_BOUND('',#583,.T.);
#268=FACE_BOUND('',#584,.T.);
#269=FACE_BOUND('',#586,.T.);
#270=FACE_BOUND('',#587,.T.);
#271=FACE_BOUND('',#599,.T.);
#272=FACE_BOUND('',#600,.T.);
#273=FACE_BOUND('',#601,.T.);
#274=FACE_BOUND('',#603,.T.);
#275=FACE_BOUND('',#604,.T.);
#276=FACE_BOUND('',#605,.T.);
#277=FACE_BOUND('',#613,.T.);
#278=FACE_BOUND('',#614,.T.);
#279=FACE_BOUND('',#616,.T.);
#280=FACE_BOUND('',#617,.T.);
#281=FACE_BOUND('',#624,.T.);
#282=FACE_BOUND('',#626,.T.);
#283=FACE_BOUND('',#631,.T.);
#284=FACE_BOUND('',#632,.T.);
#285=FACE_BOUND('',#635,.T.);
#286=FACE_BOUND('',#636,.T.);
#287=FACE_BOUND('',#639,.T.);
#288=FACE_BOUND('',#641,.T.);
#289=FACE_BOUND('',#645,.T.);
#290=FACE_BOUND('',#647,.T.);
#291=FACE_BOUND('',#650,.T.);
#292=FACE_BOUND('',#653,.T.);
#293=FACE_BOUND('',#659,.T.);
#294=FACE_BOUND('',#661,.T.);
#295=FACE_BOUND('',#664,.T.);
#296=FACE_BOUND('',#671,.T.);
#297=FACE_BOUND('',#673,.T.);
#298=FACE_BOUND('',#676,.T.);
#299=FACE_BOUND('',#683,.T.);
#300=FACE_BOUND('',#685,.T.);
#301=FACE_BOUND('',#688,.T.);
#302=FACE_BOUND('',#694,.T.);
#303=FACE_BOUND('',#696,.T.);
#304=FACE_BOUND('',#701,.T.);
#305=FACE_BOUND('',#703,.T.);
#306=FACE_BOUND('',#706,.T.);
#307=FACE_BOUND('',#713,.T.);
#308=FACE_BOUND('',#715,.T.);
#309=FACE_BOUND('',#718,.T.);
#310=FACE_BOUND('',#725,.T.);
#311=FACE_BOUND('',#727,.T.);
#312=FACE_BOUND('',#730,.T.);
#313=FACE_BOUND('',#738,.T.);
#314=FACE_BOUND('',#740,.T.);
#315=FACE_BOUND('',#744,.T.);
#316=FACE_BOUND('',#746,.T.);
#317=FACE_BOUND('',#750,.T.);
#318=FACE_BOUND('',#752,.T.);
#319=PLANE('',#2573);
#320=PLANE('',#2574);
#321=PLANE('',#2575);
#322=PLANE('',#2576);
#323=PLANE('',#2577);
#324=PLANE('',#2578);
#325=PLANE('',#2586);
#326=PLANE('',#2587);
#327=PLANE('',#2595);
#328=PLANE('',#2596);
#329=PLANE('',#2604);
#330=PLANE('',#2608);
#331=PLANE('',#2612);
#332=PLANE('',#2613);
#333=PLANE('',#2615);
#334=PLANE('',#2619);
#335=PLANE('',#2629);
#336=PLANE('',#2633);
#337=PLANE('',#2637);
#338=PLANE('',#2638);
#339=PLANE('',#2646);
#340=PLANE('',#2650);
#341=PLANE('',#2654);
#342=PLANE('',#2655);
#343=PLANE('',#2660);
#344=PLANE('',#2661);
#345=PLANE('',#2662);
#346=PLANE('',#2663);
#347=PLANE('',#2664);
#348=PLANE('',#2665);
#349=PLANE('',#2676);
#350=PLANE('',#2677);
#351=PLANE('',#2678);
#352=PLANE('',#2679);
#353=PLANE('',#2680);
#354=PLANE('',#2681);
#355=PLANE('',#2689);
#356=PLANE('',#2690);
#357=PLANE('',#2695);
#358=PLANE('',#2696);
#359=PLANE('',#2697);
#360=PLANE('',#2698);
#361=PLANE('',#2699);
#362=PLANE('',#2700);
#363=PLANE('',#2705);
#364=PLANE('',#2707);
#365=PLANE('',#2711);
#366=PLANE('',#2716);
#367=PLANE('',#2718);
#368=PLANE('',#2723);
#369=PLANE('',#2725);
#370=PLANE('',#2729);
#371=PLANE('',#2734);
#372=PLANE('',#2736);
#373=PLANE('',#2741);
#374=PLANE('',#2743);
#375=PLANE('',#2747);
#376=PLANE('',#2752);
#377=PLANE('',#2754);
#378=PLANE('',#2756);
#379=PLANE('',#2759);
#380=PLANE('',#2768);
#381=PLANE('',#2770);
#382=PLANE('',#2774);
#383=PLANE('',#2778);
#384=PLANE('',#2780);
#385=PLANE('',#2785);
#386=PLANE('',#2787);
#387=PLANE('',#2791);
#388=PLANE('',#2796);
#389=PLANE('',#2798);
#390=PLANE('',#2803);
#391=PLANE('',#2805);
#392=PLANE('',#2809);
#393=PLANE('',#2814);
#394=PLANE('',#2816);
#395=PLANE('',#2824);
#396=PLANE('',#2825);
#397=PLANE('',#2833);
#398=PLANE('',#2834);
#399=PLANE('',#2842);
#400=PLANE('',#2843);
#401=PLANE('',#2845);
#402=PLANE('',#2846);
#403=PLANE('',#2847);
#404=PLANE('',#2854);
#405=FACE_OUTER_BOUND('',#552,.T.);
#406=FACE_OUTER_BOUND('',#553,.T.);
#407=FACE_OUTER_BOUND('',#554,.T.);
#408=FACE_OUTER_BOUND('',#555,.T.);
#409=FACE_OUTER_BOUND('',#556,.T.);
#410=FACE_OUTER_BOUND('',#557,.T.);
#411=FACE_OUTER_BOUND('',#558,.T.);
#412=FACE_OUTER_BOUND('',#561,.T.);
#413=FACE_OUTER_BOUND('',#564,.T.);
#414=FACE_OUTER_BOUND('',#565,.T.);
#415=FACE_OUTER_BOUND('',#566,.T.);
#416=FACE_OUTER_BOUND('',#568,.T.);
#417=FACE_OUTER_BOUND('',#570,.T.);
#418=FACE_OUTER_BOUND('',#571,.T.);
#419=FACE_OUTER_BOUND('',#572,.T.);
#420=FACE_OUTER_BOUND('',#574,.T.);
#421=FACE_OUTER_BOUND('',#576,.T.);
#422=FACE_OUTER_BOUND('',#577,.T.);
#423=FACE_OUTER_BOUND('',#578,.T.);
#424=FACE_OUTER_BOUND('',#579,.T.);
#425=FACE_OUTER_BOUND('',#580,.T.);
#426=FACE_OUTER_BOUND('',#581,.T.);
#427=FACE_OUTER_BOUND('',#582,.T.);
#428=FACE_OUTER_BOUND('',#585,.T.);
#429=FACE_OUTER_BOUND('',#588,.T.);
#430=FACE_OUTER_BOUND('',#589,.T.);
#431=FACE_OUTER_BOUND('',#590,.T.);
#432=FACE_OUTER_BOUND('',#591,.T.);
#433=FACE_OUTER_BOUND('',#592,.T.);
#434=FACE_OUTER_BOUND('',#593,.T.);
#435=FACE_OUTER_BOUND('',#594,.T.);
#436=FACE_OUTER_BOUND('',#595,.T.);
#437=FACE_OUTER_BOUND('',#596,.T.);
#438=FACE_OUTER_BOUND('',#597,.T.);
#439=FACE_OUTER_BOUND('',#598,.T.);
#440=FACE_OUTER_BOUND('',#602,.T.);
#441=FACE_OUTER_BOUND('',#606,.T.);
#442=FACE_OUTER_BOUND('',#607,.T.);
#443=FACE_OUTER_BOUND('',#608,.T.);
#444=FACE_OUTER_BOUND('',#609,.T.);
#445=FACE_OUTER_BOUND('',#610,.T.);
#446=FACE_OUTER_BOUND('',#611,.T.);
#447=FACE_OUTER_BOUND('',#612,.T.);
#448=FACE_OUTER_BOUND('',#615,.T.);
#449=FACE_OUTER_BOUND('',#618,.T.);
#450=FACE_OUTER_BOUND('',#619,.T.);
#451=FACE_OUTER_BOUND('',#620,.T.);
#452=FACE_OUTER_BOUND('',#621,.T.);
#453=FACE_OUTER_BOUND('',#622,.T.);
#454=FACE_OUTER_BOUND('',#623,.T.);
#455=FACE_OUTER_BOUND('',#625,.T.);
#456=FACE_OUTER_BOUND('',#627,.T.);
#457=FACE_OUTER_BOUND('',#628,.T.);
#458=FACE_OUTER_BOUND('',#629,.T.);
#459=FACE_OUTER_BOUND('',#630,.T.);
#460=FACE_OUTER_BOUND('',#633,.T.);
#461=FACE_OUTER_BOUND('',#634,.T.);
#462=FACE_OUTER_BOUND('',#637,.T.);
#463=FACE_OUTER_BOUND('',#638,.T.);
#464=FACE_OUTER_BOUND('',#640,.T.);
#465=FACE_OUTER_BOUND('',#642,.T.);
#466=FACE_OUTER_BOUND('',#643,.T.);
#467=FACE_OUTER_BOUND('',#644,.T.);
#468=FACE_OUTER_BOUND('',#646,.T.);
#469=FACE_OUTER_BOUND('',#648,.T.);
#470=FACE_OUTER_BOUND('',#649,.T.);
#471=FACE_OUTER_BOUND('',#651,.T.);
#472=FACE_OUTER_BOUND('',#652,.T.);
#473=FACE_OUTER_BOUND('',#654,.T.);
#474=FACE_OUTER_BOUND('',#655,.T.);
#475=FACE_OUTER_BOUND('',#656,.T.);
#476=FACE_OUTER_BOUND('',#657,.T.);
#477=FACE_OUTER_BOUND('',#658,.T.);
#478=FACE_OUTER_BOUND('',#660,.T.);
#479=FACE_OUTER_BOUND('',#662,.T.);
#480=FACE_OUTER_BOUND('',#663,.T.);
#481=FACE_OUTER_BOUND('',#665,.T.);
#482=FACE_OUTER_BOUND('',#666,.T.);
#483=FACE_OUTER_BOUND('',#667,.T.);
#484=FACE_OUTER_BOUND('',#668,.T.);
#485=FACE_OUTER_BOUND('',#669,.T.);
#486=FACE_OUTER_BOUND('',#670,.T.);
#487=FACE_OUTER_BOUND('',#672,.T.);
#488=FACE_OUTER_BOUND('',#674,.T.);
#489=FACE_OUTER_BOUND('',#675,.T.);
#490=FACE_OUTER_BOUND('',#677,.T.);
#491=FACE_OUTER_BOUND('',#678,.T.);
#492=FACE_OUTER_BOUND('',#679,.T.);
#493=FACE_OUTER_BOUND('',#680,.T.);
#494=FACE_OUTER_BOUND('',#681,.T.);
#495=FACE_OUTER_BOUND('',#682,.T.);
#496=FACE_OUTER_BOUND('',#684,.T.);
#497=FACE_OUTER_BOUND('',#686,.T.);
#498=FACE_OUTER_BOUND('',#687,.T.);
#499=FACE_OUTER_BOUND('',#689,.T.);
#500=FACE_OUTER_BOUND('',#690,.T.);
#501=FACE_OUTER_BOUND('',#691,.T.);
#502=FACE_OUTER_BOUND('',#692,.T.);
#503=FACE_OUTER_BOUND('',#693,.T.);
#504=FACE_OUTER_BOUND('',#695,.T.);
#505=FACE_OUTER_BOUND('',#697,.T.);
#506=FACE_OUTER_BOUND('',#698,.T.);
#507=FACE_OUTER_BOUND('',#699,.T.);
#508=FACE_OUTER_BOUND('',#700,.T.);
#509=FACE_OUTER_BOUND('',#702,.T.);
#510=FACE_OUTER_BOUND('',#704,.T.);
#511=FACE_OUTER_BOUND('',#705,.T.);
#512=FACE_OUTER_BOUND('',#707,.T.);
#513=FACE_OUTER_BOUND('',#708,.T.);
#514=FACE_OUTER_BOUND('',#709,.T.);
#515=FACE_OUTER_BOUND('',#710,.T.);
#516=FACE_OUTER_BOUND('',#711,.T.);
#517=FACE_OUTER_BOUND('',#712,.T.);
#518=FACE_OUTER_BOUND('',#714,.T.);
#519=FACE_OUTER_BOUND('',#716,.T.);
#520=FACE_OUTER_BOUND('',#717,.T.);
#521=FACE_OUTER_BOUND('',#719,.T.);
#522=FACE_OUTER_BOUND('',#720,.T.);
#523=FACE_OUTER_BOUND('',#721,.T.);
#524=FACE_OUTER_BOUND('',#722,.T.);
#525=FACE_OUTER_BOUND('',#723,.T.);
#526=FACE_OUTER_BOUND('',#724,.T.);
#527=FACE_OUTER_BOUND('',#726,.T.);
#528=FACE_OUTER_BOUND('',#728,.T.);
#529=FACE_OUTER_BOUND('',#729,.T.);
#530=FACE_OUTER_BOUND('',#731,.T.);
#531=FACE_OUTER_BOUND('',#732,.T.);
#532=FACE_OUTER_BOUND('',#733,.T.);
#533=FACE_OUTER_BOUND('',#734,.T.);
#534=FACE_OUTER_BOUND('',#735,.T.);
#535=FACE_OUTER_BOUND('',#736,.T.);
#536=FACE_OUTER_BOUND('',#737,.T.);
#537=FACE_OUTER_BOUND('',#739,.T.);
#538=FACE_OUTER_BOUND('',#741,.T.);
#539=FACE_OUTER_BOUND('',#742,.T.);
#540=FACE_OUTER_BOUND('',#743,.T.);
#541=FACE_OUTER_BOUND('',#745,.T.);
#542=FACE_OUTER_BOUND('',#747,.T.);
#543=FACE_OUTER_BOUND('',#748,.T.);
#544=FACE_OUTER_BOUND('',#749,.T.);
#545=FACE_OUTER_BOUND('',#751,.T.);
#546=FACE_OUTER_BOUND('',#753,.T.);
#547=FACE_OUTER_BOUND('',#754,.T.);
#548=FACE_OUTER_BOUND('',#755,.T.);
#549=FACE_OUTER_BOUND('',#756,.T.);
#550=FACE_OUTER_BOUND('',#757,.T.);
#551=FACE_OUTER_BOUND('',#758,.T.);
#552=EDGE_LOOP('',(#1594,#1595,#1596,#1597));
#553=EDGE_LOOP('',(#1598,#1599,#1600,#1601));
#554=EDGE_LOOP('',(#1602,#1603,#1604,#1605));
#555=EDGE_LOOP('',(#1606,#1607,#1608,#1609));
#556=EDGE_LOOP('',(#1610,#1611,#1612,#1613));
#557=EDGE_LOOP('',(#1614,#1615,#1616,#1617));
#558=EDGE_LOOP('',(#1618,#1619,#1620,#1621));
#559=EDGE_LOOP('',(#1622));
#560=EDGE_LOOP('',(#1623));
#561=EDGE_LOOP('',(#1624,#1625,#1626,#1627));
#562=EDGE_LOOP('',(#1628));
#563=EDGE_LOOP('',(#1629));
#564=EDGE_LOOP('',(#1630,#1631,#1632,#1633));
#565=EDGE_LOOP('',(#1634,#1635,#1636,#1637));
#566=EDGE_LOOP('',(#1638));
#567=EDGE_LOOP('',(#1639));
#568=EDGE_LOOP('',(#1640));
#569=EDGE_LOOP('',(#1641));
#570=EDGE_LOOP('',(#1642,#1643,#1644,#1645));
#571=EDGE_LOOP('',(#1646,#1647,#1648,#1649));
#572=EDGE_LOOP('',(#1650));
#573=EDGE_LOOP('',(#1651));
#574=EDGE_LOOP('',(#1652));
#575=EDGE_LOOP('',(#1653));
#576=EDGE_LOOP('',(#1654,#1655,#1656,#1657));
#577=EDGE_LOOP('',(#1658,#1659,#1660,#1661));
#578=EDGE_LOOP('',(#1662,#1663,#1664,#1665));
#579=EDGE_LOOP('',(#1666,#1667,#1668,#1669));
#580=EDGE_LOOP('',(#1670,#1671,#1672,#1673));
#581=EDGE_LOOP('',(#1674,#1675,#1676,#1677));
#582=EDGE_LOOP('',(#1678,#1679,#1680,#1681));
#583=EDGE_LOOP('',(#1682));
#584=EDGE_LOOP('',(#1683));
#585=EDGE_LOOP('',(#1684,#1685,#1686,#1687));
#586=EDGE_LOOP('',(#1688));
#587=EDGE_LOOP('',(#1689));
#588=EDGE_LOOP('',(#1690,#1691,#1692,#1693));
#589=EDGE_LOOP('',(#1694,#1695,#1696,#1697));
#590=EDGE_LOOP('',(#1698,#1699,#1700,#1701));
#591=EDGE_LOOP('',(#1702,#1703,#1704,#1705));
#592=EDGE_LOOP('',(#1706,#1707,#1708,#1709));
#593=EDGE_LOOP('',(#1710,#1711,#1712,#1713));
#594=EDGE_LOOP('',(#1714,#1715,#1716,#1717));
#595=EDGE_LOOP('',(#1718,#1719,#1720,#1721));
#596=EDGE_LOOP('',(#1722,#1723,#1724,#1725));
#597=EDGE_LOOP('',(#1726,#1727,#1728,#1729));
#598=EDGE_LOOP('',(#1730,#1731,#1732,#1733));
#599=EDGE_LOOP('',(#1734,#1735,#1736,#1737));
#600=EDGE_LOOP('',(#1738));
#601=EDGE_LOOP('',(#1739));
#602=EDGE_LOOP('',(#1740,#1741,#1742,#1743));
#603=EDGE_LOOP('',(#1744,#1745,#1746,#1747));
#604=EDGE_LOOP('',(#1748));
#605=EDGE_LOOP('',(#1749));
#606=EDGE_LOOP('',(#1750,#1751,#1752,#1753));
#607=EDGE_LOOP('',(#1754,#1755,#1756,#1757));
#608=EDGE_LOOP('',(#1758,#1759,#1760,#1761));
#609=EDGE_LOOP('',(#1762,#1763,#1764,#1765));
#610=EDGE_LOOP('',(#1766,#1767,#1768,#1769));
#611=EDGE_LOOP('',(#1770,#1771,#1772,#1773));
#612=EDGE_LOOP('',(#1774,#1775,#1776,#1777));
#613=EDGE_LOOP('',(#1778));
#614=EDGE_LOOP('',(#1779));
#615=EDGE_LOOP('',(#1780,#1781,#1782,#1783));
#616=EDGE_LOOP('',(#1784));
#617=EDGE_LOOP('',(#1785));
#618=EDGE_LOOP('',(#1786,#1787,#1788,#1789));
#619=EDGE_LOOP('',(#1790,#1791,#1792,#1793));
#620=EDGE_LOOP('',(#1794,#1795,#1796,#1797));
#621=EDGE_LOOP('',(#1798,#1799,#1800,#1801));
#622=EDGE_LOOP('',(#1802,#1803,#1804,#1805));
#623=EDGE_LOOP('',(#1806,#1807,#1808,#1809));
#624=EDGE_LOOP('',(#1810));
#625=EDGE_LOOP('',(#1811,#1812,#1813,#1814));
#626=EDGE_LOOP('',(#1815));
#627=EDGE_LOOP('',(#1816,#1817,#1818,#1819));
#628=EDGE_LOOP('',(#1820,#1821,#1822,#1823));
#629=EDGE_LOOP('',(#1824,#1825,#1826,#1827));
#630=EDGE_LOOP('',(#1828,#1829,#1830,#1831));
#631=EDGE_LOOP('',(#1832));
#632=EDGE_LOOP('',(#1833));
#633=EDGE_LOOP('',(#1834,#1835,#1836,#1837));
#634=EDGE_LOOP('',(#1838,#1839,#1840,#1841));
#635=EDGE_LOOP('',(#1842));
#636=EDGE_LOOP('',(#1843));
#637=EDGE_LOOP('',(#1844,#1845,#1846,#1847));
#638=EDGE_LOOP('',(#1848,#1849,#1850,#1851));
#639=EDGE_LOOP('',(#1852));
#640=EDGE_LOOP('',(#1853,#1854,#1855,#1856));
#641=EDGE_LOOP('',(#1857));
#642=EDGE_LOOP('',(#1858,#1859,#1860,#1861));
#643=EDGE_LOOP('',(#1862,#1863,#1864,#1865));
#644=EDGE_LOOP('',(#1866));
#645=EDGE_LOOP('',(#1867));
#646=EDGE_LOOP('',(#1868));
#647=EDGE_LOOP('',(#1869));
#648=EDGE_LOOP('',(#1870,#1871,#1872,#1873));
#649=EDGE_LOOP('',(#1874,#1875,#1876,#1877));
#650=EDGE_LOOP('',(#1878));
#651=EDGE_LOOP('',(#1879,#1880,#1881,#1882));
#652=EDGE_LOOP('',(#1883,#1884,#1885,#1886));
#653=EDGE_LOOP('',(#1887));
#654=EDGE_LOOP('',(#1888,#1889,#1890,#1891));
#655=EDGE_LOOP('',(#1892,#1893,#1894,#1895));
#656=EDGE_LOOP('',(#1896,#1897,#1898,#1899));
#657=EDGE_LOOP('',(#1900,#1901,#1902,#1903));
#658=EDGE_LOOP('',(#1904));
#659=EDGE_LOOP('',(#1905));
#660=EDGE_LOOP('',(#1906));
#661=EDGE_LOOP('',(#1907));
#662=EDGE_LOOP('',(#1908,#1909,#1910,#1911));
#663=EDGE_LOOP('',(#1912));
#664=EDGE_LOOP('',(#1913));
#665=EDGE_LOOP('',(#1914,#1915,#1916,#1917));
#666=EDGE_LOOP('',(#1918));
#667=EDGE_LOOP('',(#1919,#1920,#1921,#1922));
#668=EDGE_LOOP('',(#1923));
#669=EDGE_LOOP('',(#1924,#1925,#1926,#1927));
#670=EDGE_LOOP('',(#1928));
#671=EDGE_LOOP('',(#1929));
#672=EDGE_LOOP('',(#1930));
#673=EDGE_LOOP('',(#1931));
#674=EDGE_LOOP('',(#1932,#1933,#1934,#1935));
#675=EDGE_LOOP('',(#1936));
#676=EDGE_LOOP('',(#1937));
#677=EDGE_LOOP('',(#1938,#1939,#1940,#1941));
#678=EDGE_LOOP('',(#1942));
#679=EDGE_LOOP('',(#1943,#1944,#1945,#1946));
#680=EDGE_LOOP('',(#1947));
#681=EDGE_LOOP('',(#1948,#1949,#1950,#1951));
#682=EDGE_LOOP('',(#1952));
#683=EDGE_LOOP('',(#1953));
#684=EDGE_LOOP('',(#1954));
#685=EDGE_LOOP('',(#1955));
#686=EDGE_LOOP('',(#1956,#1957,#1958,#1959));
#687=EDGE_LOOP('',(#1960));
#688=EDGE_LOOP('',(#1961));
#689=EDGE_LOOP('',(#1962,#1963,#1964,#1965));
#690=EDGE_LOOP('',(#1966));
#691=EDGE_LOOP('',(#1967,#1968,#1969,#1970));
#692=EDGE_LOOP('',(#1971));
#693=EDGE_LOOP('',(#1972));
#694=EDGE_LOOP('',(#1973));
#695=EDGE_LOOP('',(#1974));
#696=EDGE_LOOP('',(#1975));
#697=EDGE_LOOP('',(#1976,#1977,#1978,#1979));
#698=EDGE_LOOP('',(#1980,#1981,#1982,#1983));
#699=EDGE_LOOP('',(#1984,#1985,#1986,#1987));
#700=EDGE_LOOP('',(#1988));
#701=EDGE_LOOP('',(#1989));
#702=EDGE_LOOP('',(#1990));
#703=EDGE_LOOP('',(#1991));
#704=EDGE_LOOP('',(#1992,#1993,#1994,#1995));
#705=EDGE_LOOP('',(#1996));
#706=EDGE_LOOP('',(#1997));
#707=EDGE_LOOP('',(#1998,#1999,#2000,#2001));
#708=EDGE_LOOP('',(#2002));
#709=EDGE_LOOP('',(#2003,#2004,#2005,#2006));
#710=EDGE_LOOP('',(#2007));
#711=EDGE_LOOP('',(#2008,#2009,#2010,#2011));
#712=EDGE_LOOP('',(#2012));
#713=EDGE_LOOP('',(#2013));
#714=EDGE_LOOP('',(#2014));
#715=EDGE_LOOP('',(#2015));
#716=EDGE_LOOP('',(#2016,#2017,#2018,#2019));
#717=EDGE_LOOP('',(#2020));
#718=EDGE_LOOP('',(#2021));
#719=EDGE_LOOP('',(#2022,#2023,#2024,#2025));
#720=EDGE_LOOP('',(#2026));
#721=EDGE_LOOP('',(#2027,#2028,#2029,#2030));
#722=EDGE_LOOP('',(#2031));
#723=EDGE_LOOP('',(#2032,#2033,#2034,#2035));
#724=EDGE_LOOP('',(#2036));
#725=EDGE_LOOP('',(#2037));
#726=EDGE_LOOP('',(#2038));
#727=EDGE_LOOP('',(#2039));
#728=EDGE_LOOP('',(#2040,#2041,#2042,#2043));
#729=EDGE_LOOP('',(#2044));
#730=EDGE_LOOP('',(#2045));
#731=EDGE_LOOP('',(#2046,#2047,#2048,#2049));
#732=EDGE_LOOP('',(#2050));
#733=EDGE_LOOP('',(#2051,#2052,#2053,#2054));
#734=EDGE_LOOP('',(#2055));
#735=EDGE_LOOP('',(#2056,#2057,#2058,#2059));
#736=EDGE_LOOP('',(#2060,#2061,#2062,#2063));
#737=EDGE_LOOP('',(#2064));
#738=EDGE_LOOP('',(#2065));
#739=EDGE_LOOP('',(#2066));
#740=EDGE_LOOP('',(#2067));
#741=EDGE_LOOP('',(#2068,#2069,#2070,#2071));
#742=EDGE_LOOP('',(#2072,#2073,#2074,#2075));
#743=EDGE_LOOP('',(#2076));
#744=EDGE_LOOP('',(#2077));
#745=EDGE_LOOP('',(#2078));
#746=EDGE_LOOP('',(#2079));
#747=EDGE_LOOP('',(#2080,#2081,#2082,#2083));
#748=EDGE_LOOP('',(#2084,#2085,#2086,#2087));
#749=EDGE_LOOP('',(#2088));
#750=EDGE_LOOP('',(#2089));
#751=EDGE_LOOP('',(#2090));
#752=EDGE_LOOP('',(#2091));
#753=EDGE_LOOP('',(#2092,#2093,#2094,#2095));
#754=EDGE_LOOP('',(#2096,#2097,#2098,#2099));
#755=EDGE_LOOP('',(#2100,#2101,#2102,#2103));
#756=EDGE_LOOP('',(#2104,#2105,#2106,#2107));
#757=EDGE_LOOP('',(#2108,#2109,#2110,#2111));
#758=EDGE_LOOP('',(#2112,#2113,#2114,#2115));
#759=LINE('',#3706,#898);
#760=LINE('',#3712,#899);
#761=LINE('',#3717,#900);
#762=LINE('',#3719,#901);
#763=LINE('',#3721,#902);
#764=LINE('',#3722,#903);
#765=LINE('',#3725,#904);
#766=LINE('',#3727,#905);
#767=LINE('',#3728,#906);
#768=LINE('',#3731,#907);
#769=LINE('',#3733,#908);
#770=LINE('',#3734,#909);
#771=LINE('',#3736,#910);
#772=LINE('',#3737,#911);
#773=LINE('',#3745,#912);
#774=LINE('',#3751,#913);
#775=LINE('',#3760,#914);
#776=LINE('',#3766,#915);
#777=LINE('',#3775,#916);
#778=LINE('',#3781,#917);
#779=LINE('',#3786,#918);
#780=LINE('',#3788,#919);
#781=LINE('',#3790,#920);
#782=LINE('',#3791,#921);
#783=LINE('',#3797,#922);
#784=LINE('',#3800,#923);
#785=LINE('',#3802,#924);
#786=LINE('',#3803,#925);
#787=LINE('',#3813,#926);
#788=LINE('',#3815,#927);
#789=LINE('',#3817,#928);
#790=LINE('',#3818,#929);
#791=LINE('',#3823,#930);
#792=LINE('',#3827,#931);
#793=LINE('',#3829,#932);
#794=LINE('',#3830,#933);
#795=LINE('',#3838,#934);
#796=LINE('',#3844,#935);
#797=LINE('',#3849,#936);
#798=LINE('',#3851,#937);
#799=LINE('',#3853,#938);
#800=LINE('',#3854,#939);
#801=LINE('',#3860,#940);
#802=LINE('',#3863,#941);
#803=LINE('',#3865,#942);
#804=LINE('',#3866,#943);
#805=LINE('',#3877,#944);
#806=LINE('',#3883,#945);
#807=LINE('',#3888,#946);
#808=LINE('',#3890,#947);
#809=LINE('',#3892,#948);
#810=LINE('',#3893,#949);
#811=LINE('',#3899,#950);
#812=LINE('',#3902,#951);
#813=LINE('',#3904,#952);
#814=LINE('',#3905,#953);
#815=LINE('',#3916,#954);
#816=LINE('',#3921,#955);
#817=LINE('',#3923,#956);
#818=LINE('',#3925,#957);
#819=LINE('',#3926,#958);
#820=LINE('',#3929,#959);
#821=LINE('',#3931,#960);
#822=LINE('',#3932,#961);
#823=LINE('',#3935,#962);
#824=LINE('',#3937,#963);
#825=LINE('',#3938,#964);
#826=LINE('',#3940,#965);
#827=LINE('',#3941,#966);
#828=LINE('',#3949,#967);
#829=LINE('',#3955,#968);
#830=LINE('',#3961,#969);
#831=LINE('',#3966,#970);
#832=LINE('',#3968,#971);
#833=LINE('',#3970,#972);
#834=LINE('',#3971,#973);
#835=LINE('',#3974,#974);
#836=LINE('',#3976,#975);
#837=LINE('',#3977,#976);
#838=LINE('',#3980,#977);
#839=LINE('',#3982,#978);
#840=LINE('',#3983,#979);
#841=LINE('',#3985,#980);
#842=LINE('',#3986,#981);
#843=LINE('',#3994,#982);
#844=LINE('',#4000,#983);
#845=LINE('',#4009,#984);
#846=LINE('',#4014,#985);
#847=LINE('',#4016,#986);
#848=LINE('',#4018,#987);
#849=LINE('',#4019,#988);
#850=LINE('',#4022,#989);
#851=LINE('',#4024,#990);
#852=LINE('',#4025,#991);
#853=LINE('',#4028,#992);
#854=LINE('',#4030,#993);
#855=LINE('',#4031,#994);
#856=LINE('',#4033,#995);
#857=LINE('',#4034,#996);
#858=LINE('',#4042,#997);
#859=LINE('',#4053,#998);
#860=LINE('',#4061,#999);
#861=LINE('',#4065,#1000);
#862=LINE('',#4072,#1001);
#863=LINE('',#4083,#1002);
#864=LINE('',#4091,#1003);
#865=LINE('',#4095,#1004);
#866=LINE('',#4102,#1005);
#867=LINE('',#4113,#1006);
#868=LINE('',#4121,#1007);
#869=LINE('',#4125,#1008);
#870=LINE('',#4139,#1009);
#871=LINE('',#4142,#1010);
#872=LINE('',#4148,#1011);
#873=LINE('',#4159,#1012);
#874=LINE('',#4165,#1013);
#875=LINE('',#4169,#1014);
#876=LINE('',#4176,#1015);
#877=LINE('',#4187,#1016);
#878=LINE('',#4195,#1017);
#879=LINE('',#4199,#1018);
#880=LINE('',#4206,#1019);
#881=LINE('',#4217,#1020);
#882=LINE('',#4225,#1021);
#883=LINE('',#4229,#1022);
#884=LINE('',#4236,#1023);
#885=LINE('',#4242,#1024);
#886=LINE('',#4251,#1025);
#887=LINE('',#4257,#1026);
#888=LINE('',#4266,#1027);
#889=LINE('',#4272,#1028);
#890=LINE('',#4280,#1029);
#891=LINE('',#4282,#1030);
#892=LINE('',#4284,#1031);
#893=LINE('',#4285,#1032);
#894=LINE('',#4289,#1033);
#895=LINE('',#4291,#1034);
#896=LINE('',#4293,#1035);
#897=LINE('',#4294,#1036);
#898=VECTOR('',#2905,5.);
#899=VECTOR('',#2912,5.);
#900=VECTOR('',#2917,10.);
#901=VECTOR('',#2918,10.);
#902=VECTOR('',#2919,10.);
#903=VECTOR('',#2920,10.);
#904=VECTOR('',#2923,10.);
#905=VECTOR('',#2924,10.);
#906=VECTOR('',#2925,10.);
#907=VECTOR('',#2928,10.);
#908=VECTOR('',#2929,10.);
#909=VECTOR('',#2930,10.);
#910=VECTOR('',#2933,10.);
#911=VECTOR('',#2934,10.);
#912=VECTOR('',#2945,5.);
#913=VECTOR('',#2952,12.);
#914=VECTOR('',#2965,5.);
#915=VECTOR('',#2972,12.);
#916=VECTOR('',#2985,7.);
#917=VECTOR('',#2992,7.);
#918=VECTOR('',#2997,10.);
#919=VECTOR('',#2998,10.);
#920=VECTOR('',#2999,10.);
#921=VECTOR('',#3000,10.);
#922=VECTOR('',#3007,10.);
#923=VECTOR('',#3010,10.);
#924=VECTOR('',#3011,10.);
#925=VECTOR('',#3012,10.);
#926=VECTOR('',#3027,10.);
#927=VECTOR('',#3028,10.);
#928=VECTOR('',#3029,10.);
#929=VECTOR('',#3030,10.);
#930=VECTOR('',#3035,10.);
#931=VECTOR('',#3040,10.);
#932=VECTOR('',#3041,10.);
#933=VECTOR('',#3042,10.);
#934=VECTOR('',#3053,7.);
#935=VECTOR('',#3060,7.);
#936=VECTOR('',#3065,10.);
#937=VECTOR('',#3066,10.);
#938=VECTOR('',#3067,10.);
#939=VECTOR('',#3068,10.);
#940=VECTOR('',#3075,10.);
#941=VECTOR('',#3078,10.);
#942=VECTOR('',#3079,10.);
#943=VECTOR('',#3080,10.);
#944=VECTOR('',#3097,7.);
#945=VECTOR('',#3104,7.);
#946=VECTOR('',#3109,10.);
#947=VECTOR('',#3110,10.);
#948=VECTOR('',#3111,10.);
#949=VECTOR('',#3112,10.);
#950=VECTOR('',#3119,10.);
#951=VECTOR('',#3122,10.);
#952=VECTOR('',#3123,10.);
#953=VECTOR('',#3124,10.);
#954=VECTOR('',#3141,5.);
#955=VECTOR('',#3146,10.);
#956=VECTOR('',#3147,10.);
#957=VECTOR('',#3148,10.);
#958=VECTOR('',#3149,10.);
#959=VECTOR('',#3152,10.);
#960=VECTOR('',#3153,10.);
#961=VECTOR('',#3154,10.);
#962=VECTOR('',#3157,10.);
#963=VECTOR('',#3158,10.);
#964=VECTOR('',#3159,10.);
#965=VECTOR('',#3162,10.);
#966=VECTOR('',#3163,10.);
#967=VECTOR('',#3174,5.);
#968=VECTOR('',#3181,5.);
#969=VECTOR('',#3188,5.);
#970=VECTOR('',#3193,10.);
#971=VECTOR('',#3194,10.);
#972=VECTOR('',#3195,10.);
#973=VECTOR('',#3196,10.);
#974=VECTOR('',#3199,10.);
#975=VECTOR('',#3200,10.);
#976=VECTOR('',#3201,10.);
#977=VECTOR('',#3204,10.);
#978=VECTOR('',#3205,10.);
#979=VECTOR('',#3206,10.);
#980=VECTOR('',#3209,10.);
#981=VECTOR('',#3210,10.);
#982=VECTOR('',#3221,5.);
#983=VECTOR('',#3228,12.);
#984=VECTOR('',#3241,5.);
#985=VECTOR('',#3246,10.);
#986=VECTOR('',#3247,10.);
#987=VECTOR('',#3248,10.);
#988=VECTOR('',#3249,10.);
#989=VECTOR('',#3252,10.);
#990=VECTOR('',#3253,10.);
#991=VECTOR('',#3254,10.);
#992=VECTOR('',#3257,10.);
#993=VECTOR('',#3258,10.);
#994=VECTOR('',#3259,10.);
#995=VECTOR('',#3262,10.);
#996=VECTOR('',#3263,10.);
#997=VECTOR('',#3274,4.);
#998=VECTOR('',#3289,5.);
#999=VECTOR('',#3298,8.);
#1000=VECTOR('',#3305,5.);
#1001=VECTOR('',#3314,4.);
#1002=VECTOR('',#3329,5.);
#1003=VECTOR('',#3338,8.);
#1004=VECTOR('',#3345,5.);
#1005=VECTOR('',#3354,4.);
#1006=VECTOR('',#3369,5.);
#1007=VECTOR('',#3378,8.);
#1008=VECTOR('',#3385,5.);
#1009=VECTOR('',#3404,7.);
#1010=VECTOR('',#3407,5.);
#1011=VECTOR('',#3414,4.);
#1012=VECTOR('',#3429,5.);
#1013=VECTOR('',#3436,8.);
#1014=VECTOR('',#3443,5.);
#1015=VECTOR('',#3452,4.);
#1016=VECTOR('',#3467,5.);
#1017=VECTOR('',#3476,8.);
#1018=VECTOR('',#3483,5.);
#1019=VECTOR('',#3492,4.);
#1020=VECTOR('',#3507,5.);
#1021=VECTOR('',#3516,8.);
#1022=VECTOR('',#3523,5.);
#1023=VECTOR('',#3532,5.);
#1024=VECTOR('',#3539,7.);
#1025=VECTOR('',#3552,5.);
#1026=VECTOR('',#3559,7.);
#1027=VECTOR('',#3572,5.);
#1028=VECTOR('',#3579,10.);
#1029=VECTOR('',#3590,10.);
#1030=VECTOR('',#3591,10.);
#1031=VECTOR('',#3592,10.);
#1032=VECTOR('',#3593,10.);
#1033=VECTOR('',#3596,10.);
#1034=VECTOR('',#3597,10.);
#1035=VECTOR('',#3598,10.);
#1036=VECTOR('',#3599,10.);
#1037=CIRCLE('',#2568,5.);
#1038=CIRCLE('',#2569,5.);
#1039=CIRCLE('',#2571,5.);
#1040=CIRCLE('',#2572,5.);
#1041=CIRCLE('',#2581,5.);
#1042=CIRCLE('',#2582,5.);
#1043=CIRCLE('',#2584,12.);
#1044=CIRCLE('',#2585,12.);
#1045=CIRCLE('',#2590,5.);
#1046=CIRCLE('',#2591,5.);
#1047=CIRCLE('',#2593,12.);
#1048=CIRCLE('',#2594,12.);
#1049=CIRCLE('',#2599,7.);
#1050=CIRCLE('',#2600,7.);
#1051=CIRCLE('',#2602,7.);
#1052=CIRCLE('',#2603,7.);
#1053=CIRCLE('',#2606,12.);
#1054=CIRCLE('',#2607,12.);
#1055=CIRCLE('',#2610,12.);
#1056=CIRCLE('',#2611,12.);
#1057=CIRCLE('',#2617,7.);
#1058=CIRCLE('',#2618,7.);
#1059=CIRCLE('',#2621,7.);
#1060=CIRCLE('',#2622,7.);
#1061=CIRCLE('',#2624,7.);
#1062=CIRCLE('',#2625,7.);
#1063=CIRCLE('',#2627,7.);
#1064=CIRCLE('',#2628,7.);
#1065=CIRCLE('',#2631,15.);
#1066=CIRCLE('',#2632,15.);
#1067=CIRCLE('',#2635,15.);
#1068=CIRCLE('',#2636,15.);
#1069=CIRCLE('',#2641,7.);
#1070=CIRCLE('',#2642,7.);
#1071=CIRCLE('',#2644,7.);
#1072=CIRCLE('',#2645,7.);
#1073=CIRCLE('',#2648,12.);
#1074=CIRCLE('',#2649,12.);
#1075=CIRCLE('',#2652,12.);
#1076=CIRCLE('',#2653,12.);
#1077=CIRCLE('',#2658,5.);
#1078=CIRCLE('',#2659,5.);
#1079=CIRCLE('',#2668,5.);
#1080=CIRCLE('',#2669,5.);
#1081=CIRCLE('',#2671,5.);
#1082=CIRCLE('',#2672,5.);
#1083=CIRCLE('',#2674,5.);
#1084=CIRCLE('',#2675,5.);
#1085=CIRCLE('',#2684,5.);
#1086=CIRCLE('',#2685,5.);
#1087=CIRCLE('',#2687,12.);
#1088=CIRCLE('',#2688,12.);
#1089=CIRCLE('',#2693,5.);
#1090=CIRCLE('',#2694,5.);
#1091=CIRCLE('',#2703,4.);
#1092=CIRCLE('',#2704,4.);
#1093=CIRCLE('',#2706,5.);
#1094=CIRCLE('',#2708,5.);
#1095=CIRCLE('',#2710,5.);
#1096=CIRCLE('',#2712,8.);
#1097=CIRCLE('',#2713,5.);
#1098=CIRCLE('',#2715,8.);
#1099=CIRCLE('',#2721,4.);
#1100=CIRCLE('',#2722,4.);
#1101=CIRCLE('',#2724,5.);
#1102=CIRCLE('',#2726,5.);
#1103=CIRCLE('',#2728,5.);
#1104=CIRCLE('',#2730,8.);
#1105=CIRCLE('',#2731,5.);
#1106=CIRCLE('',#2733,8.);
#1107=CIRCLE('',#2739,4.);
#1108=CIRCLE('',#2740,4.);
#1109=CIRCLE('',#2742,5.);
#1110=CIRCLE('',#2744,5.);
#1111=CIRCLE('',#2746,5.);
#1112=CIRCLE('',#2748,8.);
#1113=CIRCLE('',#2749,5.);
#1114=CIRCLE('',#2751,8.);
#1115=CIRCLE('',#2757,7.);
#1116=CIRCLE('',#2758,5.);
#1117=CIRCLE('',#2760,7.);
#1118=CIRCLE('',#2761,5.);
#1119=CIRCLE('',#2764,5.);
#1120=CIRCLE('',#2766,4.);
#1121=CIRCLE('',#2767,4.);
#1122=CIRCLE('',#2769,5.);
#1123=CIRCLE('',#2771,5.);
#1124=CIRCLE('',#2773,5.);
#1125=CIRCLE('',#2775,8.);
#1126=CIRCLE('',#2777,8.);
#1127=CIRCLE('',#2783,4.);
#1128=CIRCLE('',#2784,4.);
#1129=CIRCLE('',#2786,5.);
#1130=CIRCLE('',#2788,5.);
#1131=CIRCLE('',#2790,5.);
#1132=CIRCLE('',#2792,8.);
#1133=CIRCLE('',#2793,5.);
#1134=CIRCLE('',#2795,8.);
#1135=CIRCLE('',#2801,4.);
#1136=CIRCLE('',#2802,4.);
#1137=CIRCLE('',#2804,5.);
#1138=CIRCLE('',#2806,5.);
#1139=CIRCLE('',#2808,5.);
#1140=CIRCLE('',#2810,8.);
#1141=CIRCLE('',#2811,5.);
#1142=CIRCLE('',#2813,8.);
#1143=CIRCLE('',#2819,5.);
#1144=CIRCLE('',#2820,5.);
#1145=CIRCLE('',#2822,7.);
#1146=CIRCLE('',#2823,7.);
#1147=CIRCLE('',#2828,5.);
#1148=CIRCLE('',#2829,5.);
#1149=CIRCLE('',#2831,7.);
#1150=CIRCLE('',#2832,7.);
#1151=CIRCLE('',#2837,5.);
#1152=CIRCLE('',#2838,5.);
#1153=CIRCLE('',#2840,10.);
#1154=CIRCLE('',#2841,10.);
#1155=CIRCLE('',#2848,8.);
#1156=CIRCLE('',#2849,4.);
#1157=CIRCLE('',#2851,4.);
#1158=CIRCLE('',#2853,8.);
#1159=VERTEX_POINT('',#3703);
#1160=VERTEX_POINT('',#3705);
#1161=VERTEX_POINT('',#3709);
#1162=VERTEX_POINT('',#3711);
#1163=VERTEX_POINT('',#3715);
#1164=VERTEX_POINT('',#3716);
#1165=VERTEX_POINT('',#3718);
#1166=VERTEX_POINT('',#3720);
#1167=VERTEX_POINT('',#3724);
#1168=VERTEX_POINT('',#3726);
#1169=VERTEX_POINT('',#3730);
#1170=VERTEX_POINT('',#3732);
#1171=VERTEX_POINT('',#3742);
#1172=VERTEX_POINT('',#3744);
#1173=VERTEX_POINT('',#3748);
#1174=VERTEX_POINT('',#3750);
#1175=VERTEX_POINT('',#3757);
#1176=VERTEX_POINT('',#3759);
#1177=VERTEX_POINT('',#3763);
#1178=VERTEX_POINT('',#3765);
#1179=VERTEX_POINT('',#3772);
#1180=VERTEX_POINT('',#3774);
#1181=VERTEX_POINT('',#3778);
#1182=VERTEX_POINT('',#3780);
#1183=VERTEX_POINT('',#3784);
#1184=VERTEX_POINT('',#3785);
#1185=VERTEX_POINT('',#3787);
#1186=VERTEX_POINT('',#3789);
#1187=VERTEX_POINT('',#3793);
#1188=VERTEX_POINT('',#3795);
#1189=VERTEX_POINT('',#3799);
#1190=VERTEX_POINT('',#3801);
#1191=VERTEX_POINT('',#3811);
#1192=VERTEX_POINT('',#3812);
#1193=VERTEX_POINT('',#3814);
#1194=VERTEX_POINT('',#3816);
#1195=VERTEX_POINT('',#3820);
#1196=VERTEX_POINT('',#3822);
#1197=VERTEX_POINT('',#3826);
#1198=VERTEX_POINT('',#3828);
#1199=VERTEX_POINT('',#3835);
#1200=VERTEX_POINT('',#3837);
#1201=VERTEX_POINT('',#3841);
#1202=VERTEX_POINT('',#3843);
#1203=VERTEX_POINT('',#3847);
#1204=VERTEX_POINT('',#3848);
#1205=VERTEX_POINT('',#3850);
#1206=VERTEX_POINT('',#3852);
#1207=VERTEX_POINT('',#3856);
#1208=VERTEX_POINT('',#3858);
#1209=VERTEX_POINT('',#3862);
#1210=VERTEX_POINT('',#3864);
#1211=VERTEX_POINT('',#3874);
#1212=VERTEX_POINT('',#3876);
#1213=VERTEX_POINT('',#3880);
#1214=VERTEX_POINT('',#3882);
#1215=VERTEX_POINT('',#3886);
#1216=VERTEX_POINT('',#3887);
#1217=VERTEX_POINT('',#3889);
#1218=VERTEX_POINT('',#3891);
#1219=VERTEX_POINT('',#3895);
#1220=VERTEX_POINT('',#3897);
#1221=VERTEX_POINT('',#3901);
#1222=VERTEX_POINT('',#3903);
#1223=VERTEX_POINT('',#3913);
#1224=VERTEX_POINT('',#3915);
#1225=VERTEX_POINT('',#3919);
#1226=VERTEX_POINT('',#3920);
#1227=VERTEX_POINT('',#3922);
#1228=VERTEX_POINT('',#3924);
#1229=VERTEX_POINT('',#3928);
#1230=VERTEX_POINT('',#3930);
#1231=VERTEX_POINT('',#3934);
#1232=VERTEX_POINT('',#3936);
#1233=VERTEX_POINT('',#3946);
#1234=VERTEX_POINT('',#3948);
#1235=VERTEX_POINT('',#3952);
#1236=VERTEX_POINT('',#3954);
#1237=VERTEX_POINT('',#3958);
#1238=VERTEX_POINT('',#3960);
#1239=VERTEX_POINT('',#3964);
#1240=VERTEX_POINT('',#3965);
#1241=VERTEX_POINT('',#3967);
#1242=VERTEX_POINT('',#3969);
#1243=VERTEX_POINT('',#3973);
#1244=VERTEX_POINT('',#3975);
#1245=VERTEX_POINT('',#3979);
#1246=VERTEX_POINT('',#3981);
#1247=VERTEX_POINT('',#3991);
#1248=VERTEX_POINT('',#3993);
#1249=VERTEX_POINT('',#3997);
#1250=VERTEX_POINT('',#3999);
#1251=VERTEX_POINT('',#4006);
#1252=VERTEX_POINT('',#4008);
#1253=VERTEX_POINT('',#4012);
#1254=VERTEX_POINT('',#4013);
#1255=VERTEX_POINT('',#4015);
#1256=VERTEX_POINT('',#4017);
#1257=VERTEX_POINT('',#4021);
#1258=VERTEX_POINT('',#4023);
#1259=VERTEX_POINT('',#4027);
#1260=VERTEX_POINT('',#4029);
#1261=VERTEX_POINT('',#4039);
#1262=VERTEX_POINT('',#4041);
#1263=VERTEX_POINT('',#4045);
#1264=VERTEX_POINT('',#4048);
#1265=VERTEX_POINT('',#4051);
#1266=VERTEX_POINT('',#4055);
#1267=VERTEX_POINT('',#4057);
#1268=VERTEX_POINT('',#4060);
#1269=VERTEX_POINT('',#4069);
#1270=VERTEX_POINT('',#4071);
#1271=VERTEX_POINT('',#4075);
#1272=VERTEX_POINT('',#4078);
#1273=VERTEX_POINT('',#4081);
#1274=VERTEX_POINT('',#4085);
#1275=VERTEX_POINT('',#4087);
#1276=VERTEX_POINT('',#4090);
#1277=VERTEX_POINT('',#4099);
#1278=VERTEX_POINT('',#4101);
#1279=VERTEX_POINT('',#4105);
#1280=VERTEX_POINT('',#4108);
#1281=VERTEX_POINT('',#4111);
#1282=VERTEX_POINT('',#4115);
#1283=VERTEX_POINT('',#4117);
#1284=VERTEX_POINT('',#4120);
#1285=VERTEX_POINT('',#4129);
#1286=VERTEX_POINT('',#4131);
#1287=VERTEX_POINT('',#4134);
#1288=VERTEX_POINT('',#4136);
#1289=VERTEX_POINT('',#4141);
#1290=VERTEX_POINT('',#4145);
#1291=VERTEX_POINT('',#4147);
#1292=VERTEX_POINT('',#4151);
#1293=VERTEX_POINT('',#4154);
#1294=VERTEX_POINT('',#4157);
#1295=VERTEX_POINT('',#4161);
#1296=VERTEX_POINT('',#4164);
#1297=VERTEX_POINT('',#4173);
#1298=VERTEX_POINT('',#4175);
#1299=VERTEX_POINT('',#4179);
#1300=VERTEX_POINT('',#4182);
#1301=VERTEX_POINT('',#4185);
#1302=VERTEX_POINT('',#4189);
#1303=VERTEX_POINT('',#4191);
#1304=VERTEX_POINT('',#4194);
#1305=VERTEX_POINT('',#4203);
#1306=VERTEX_POINT('',#4205);
#1307=VERTEX_POINT('',#4209);
#1308=VERTEX_POINT('',#4212);
#1309=VERTEX_POINT('',#4215);
#1310=VERTEX_POINT('',#4219);
#1311=VERTEX_POINT('',#4221);
#1312=VERTEX_POINT('',#4224);
#1313=VERTEX_POINT('',#4233);
#1314=VERTEX_POINT('',#4235);
#1315=VERTEX_POINT('',#4239);
#1316=VERTEX_POINT('',#4241);
#1317=VERTEX_POINT('',#4248);
#1318=VERTEX_POINT('',#4250);
#1319=VERTEX_POINT('',#4254);
#1320=VERTEX_POINT('',#4256);
#1321=VERTEX_POINT('',#4263);
#1322=VERTEX_POINT('',#4265);
#1323=VERTEX_POINT('',#4269);
#1324=VERTEX_POINT('',#4271);
#1325=VERTEX_POINT('',#4278);
#1326=VERTEX_POINT('',#4279);
#1327=VERTEX_POINT('',#4281);
#1328=VERTEX_POINT('',#4283);
#1329=VERTEX_POINT('',#4287);
#1330=VERTEX_POINT('',#4288);
#1331=VERTEX_POINT('',#4290);
#1332=VERTEX_POINT('',#4292);
#1333=EDGE_CURVE('',#1159,#1159,#1037,.T.);
#1334=EDGE_CURVE('',#1159,#1160,#759,.T.);
#1335=EDGE_CURVE('',#1160,#1160,#1038,.T.);
#1336=EDGE_CURVE('',#1161,#1161,#1039,.T.);
#1337=EDGE_CURVE('',#1161,#1162,#760,.T.);
#1338=EDGE_CURVE('',#1162,#1162,#1040,.T.);
#1339=EDGE_CURVE('',#1163,#1164,#761,.F.);
#1340=EDGE_CURVE('',#1164,#1165,#762,.T.);
#1341=EDGE_CURVE('',#1166,#1165,#763,.F.);
#1342=EDGE_CURVE('',#1163,#1166,#764,.F.);
#1343=EDGE_CURVE('',#1167,#1163,#765,.F.);
#1344=EDGE_CURVE('',#1168,#1166,#766,.F.);
#1345=EDGE_CURVE('',#1167,#1168,#767,.F.);
#1346=EDGE_CURVE('',#1169,#1167,#768,.F.);
#1347=EDGE_CURVE('',#1170,#1168,#769,.F.);
#1348=EDGE_CURVE('',#1169,#1170,#770,.T.);
#1349=EDGE_CURVE('',#1164,#1169,#771,.F.);
#1350=EDGE_CURVE('',#1165,#1170,#772,.F.);
#1351=EDGE_CURVE('',#1171,#1171,#1041,.T.);
#1352=EDGE_CURVE('',#1171,#1172,#773,.T.);
#1353=EDGE_CURVE('',#1172,#1172,#1042,.T.);
#1354=EDGE_CURVE('',#1173,#1173,#1043,.T.);
#1355=EDGE_CURVE('',#1173,#1174,#774,.T.);
#1356=EDGE_CURVE('',#1174,#1174,#1044,.T.);
#1357=EDGE_CURVE('',#1175,#1175,#1045,.T.);
#1358=EDGE_CURVE('',#1175,#1176,#775,.T.);
#1359=EDGE_CURVE('',#1176,#1176,#1046,.T.);
#1360=EDGE_CURVE('',#1177,#1177,#1047,.T.);
#1361=EDGE_CURVE('',#1177,#1178,#776,.T.);
#1362=EDGE_CURVE('',#1178,#1178,#1048,.T.);
#1363=EDGE_CURVE('',#1179,#1179,#1049,.T.);
#1364=EDGE_CURVE('',#1179,#1180,#777,.T.);
#1365=EDGE_CURVE('',#1180,#1180,#1050,.T.);
#1366=EDGE_CURVE('',#1181,#1181,#1051,.T.);
#1367=EDGE_CURVE('',#1181,#1182,#778,.T.);
#1368=EDGE_CURVE('',#1182,#1182,#1052,.T.);
#1369=EDGE_CURVE('',#1183,#1184,#779,.T.);
#1370=EDGE_CURVE('',#1184,#1185,#780,.T.);
#1371=EDGE_CURVE('',#1186,#1185,#781,.T.);
#1372=EDGE_CURVE('',#1183,#1186,#782,.T.);
#1373=EDGE_CURVE('',#1187,#1183,#1053,.T.);
#1374=EDGE_CURVE('',#1188,#1186,#1054,.T.);
#1375=EDGE_CURVE('',#1187,#1188,#783,.T.);
#1376=EDGE_CURVE('',#1189,#1187,#784,.T.);
#1377=EDGE_CURVE('',#1190,#1188,#785,.T.);
#1378=EDGE_CURVE('',#1189,#1190,#786,.T.);
#1379=EDGE_CURVE('',#1184,#1189,#1055,.T.);
#1380=EDGE_CURVE('',#1185,#1190,#1056,.T.);
#1381=EDGE_CURVE('',#1191,#1192,#787,.T.);
#1382=EDGE_CURVE('',#1191,#1193,#788,.T.);
#1383=EDGE_CURVE('',#1194,#1193,#789,.T.);
#1384=EDGE_CURVE('',#1192,#1194,#790,.T.);
#1385=EDGE_CURVE('',#1195,#1191,#1057,.T.);
#1386=EDGE_CURVE('',#1195,#1196,#791,.T.);
#1387=EDGE_CURVE('',#1193,#1196,#1058,.T.);
#1388=EDGE_CURVE('',#1197,#1195,#792,.T.);
#1389=EDGE_CURVE('',#1197,#1198,#793,.T.);
#1390=EDGE_CURVE('',#1196,#1198,#794,.T.);
#1391=EDGE_CURVE('',#1192,#1197,#1059,.T.);
#1392=EDGE_CURVE('',#1198,#1194,#1060,.T.);
#1393=EDGE_CURVE('',#1199,#1199,#1061,.T.);
#1394=EDGE_CURVE('',#1199,#1200,#795,.T.);
#1395=EDGE_CURVE('',#1200,#1200,#1062,.T.);
#1396=EDGE_CURVE('',#1201,#1201,#1063,.T.);
#1397=EDGE_CURVE('',#1201,#1202,#796,.T.);
#1398=EDGE_CURVE('',#1202,#1202,#1064,.T.);
#1399=EDGE_CURVE('',#1203,#1204,#797,.T.);
#1400=EDGE_CURVE('',#1204,#1205,#798,.T.);
#1401=EDGE_CURVE('',#1206,#1205,#799,.T.);
#1402=EDGE_CURVE('',#1203,#1206,#800,.T.);
#1403=EDGE_CURVE('',#1207,#1203,#1065,.T.);
#1404=EDGE_CURVE('',#1208,#1206,#1066,.T.);
#1405=EDGE_CURVE('',#1207,#1208,#801,.T.);
#1406=EDGE_CURVE('',#1209,#1207,#802,.T.);
#1407=EDGE_CURVE('',#1210,#1208,#803,.T.);
#1408=EDGE_CURVE('',#1209,#1210,#804,.T.);
#1409=EDGE_CURVE('',#1204,#1209,#1067,.T.);
#1410=EDGE_CURVE('',#1205,#1210,#1068,.T.);
#1411=EDGE_CURVE('',#1211,#1211,#1069,.T.);
#1412=EDGE_CURVE('',#1211,#1212,#805,.T.);
#1413=EDGE_CURVE('',#1212,#1212,#1070,.T.);
#1414=EDGE_CURVE('',#1213,#1213,#1071,.T.);
#1415=EDGE_CURVE('',#1213,#1214,#806,.T.);
#1416=EDGE_CURVE('',#1214,#1214,#1072,.T.);
#1417=EDGE_CURVE('',#1215,#1216,#807,.T.);
#1418=EDGE_CURVE('',#1216,#1217,#808,.T.);
#1419=EDGE_CURVE('',#1218,#1217,#809,.T.);
#1420=EDGE_CURVE('',#1215,#1218,#810,.T.);
#1421=EDGE_CURVE('',#1219,#1215,#1073,.T.);
#1422=EDGE_CURVE('',#1220,#1218,#1074,.T.);
#1423=EDGE_CURVE('',#1219,#1220,#811,.T.);
#1424=EDGE_CURVE('',#1221,#1219,#812,.T.);
#1425=EDGE_CURVE('',#1222,#1220,#813,.T.);
#1426=EDGE_CURVE('',#1221,#1222,#814,.T.);
#1427=EDGE_CURVE('',#1216,#1221,#1075,.T.);
#1428=EDGE_CURVE('',#1217,#1222,#1076,.T.);
#1429=EDGE_CURVE('',#1223,#1223,#1077,.T.);
#1430=EDGE_CURVE('',#1223,#1224,#815,.T.);
#1431=EDGE_CURVE('',#1224,#1224,#1078,.T.);
#1432=EDGE_CURVE('',#1225,#1226,#816,.T.);
#1433=EDGE_CURVE('',#1226,#1227,#817,.T.);
#1434=EDGE_CURVE('',#1228,#1227,#818,.T.);
#1435=EDGE_CURVE('',#1225,#1228,#819,.T.);
#1436=EDGE_CURVE('',#1229,#1225,#820,.T.);
#1437=EDGE_CURVE('',#1230,#1228,#821,.T.);
#1438=EDGE_CURVE('',#1229,#1230,#822,.T.);
#1439=EDGE_CURVE('',#1231,#1229,#823,.T.);
#1440=EDGE_CURVE('',#1232,#1230,#824,.T.);
#1441=EDGE_CURVE('',#1231,#1232,#825,.T.);
#1442=EDGE_CURVE('',#1226,#1231,#826,.T.);
#1443=EDGE_CURVE('',#1227,#1232,#827,.T.);
#1444=EDGE_CURVE('',#1233,#1233,#1079,.T.);
#1445=EDGE_CURVE('',#1233,#1234,#828,.T.);
#1446=EDGE_CURVE('',#1234,#1234,#1080,.T.);
#1447=EDGE_CURVE('',#1235,#1235,#1081,.T.);
#1448=EDGE_CURVE('',#1235,#1236,#829,.T.);
#1449=EDGE_CURVE('',#1236,#1236,#1082,.T.);
#1450=EDGE_CURVE('',#1237,#1237,#1083,.T.);
#1451=EDGE_CURVE('',#1237,#1238,#830,.T.);
#1452=EDGE_CURVE('',#1238,#1238,#1084,.T.);
#1453=EDGE_CURVE('',#1239,#1240,#831,.T.);
#1454=EDGE_CURVE('',#1240,#1241,#832,.T.);
#1455=EDGE_CURVE('',#1242,#1241,#833,.T.);
#1456=EDGE_CURVE('',#1239,#1242,#834,.T.);
#1457=EDGE_CURVE('',#1243,#1239,#835,.T.);
#1458=EDGE_CURVE('',#1244,#1242,#836,.T.);
#1459=EDGE_CURVE('',#1243,#1244,#837,.T.);
#1460=EDGE_CURVE('',#1245,#1243,#838,.T.);
#1461=EDGE_CURVE('',#1246,#1244,#839,.T.);
#1462=EDGE_CURVE('',#1245,#1246,#840,.T.);
#1463=EDGE_CURVE('',#1240,#1245,#841,.T.);
#1464=EDGE_CURVE('',#1241,#1246,#842,.T.);
#1465=EDGE_CURVE('',#1247,#1247,#1085,.T.);
#1466=EDGE_CURVE('',#1247,#1248,#843,.T.);
#1467=EDGE_CURVE('',#1248,#1248,#1086,.T.);
#1468=EDGE_CURVE('',#1249,#1249,#1087,.T.);
#1469=EDGE_CURVE('',#1249,#1250,#844,.T.);
#1470=EDGE_CURVE('',#1250,#1250,#1088,.T.);
#1471=EDGE_CURVE('',#1251,#1251,#1089,.T.);
#1472=EDGE_CURVE('',#1251,#1252,#845,.T.);
#1473=EDGE_CURVE('',#1252,#1252,#1090,.T.);
#1474=EDGE_CURVE('',#1253,#1254,#846,.T.);
#1475=EDGE_CURVE('',#1254,#1255,#847,.T.);
#1476=EDGE_CURVE('',#1256,#1255,#848,.T.);
#1477=EDGE_CURVE('',#1253,#1256,#849,.T.);
#1478=EDGE_CURVE('',#1257,#1253,#850,.T.);
#1479=EDGE_CURVE('',#1258,#1256,#851,.T.);
#1480=EDGE_CURVE('',#1257,#1258,#852,.T.);
#1481=EDGE_CURVE('',#1259,#1257,#853,.T.);
#1482=EDGE_CURVE('',#1260,#1258,#854,.T.);
#1483=EDGE_CURVE('',#1259,#1260,#855,.T.);
#1484=EDGE_CURVE('',#1254,#1259,#856,.T.);
#1485=EDGE_CURVE('',#1255,#1260,#857,.T.);
#1486=EDGE_CURVE('',#1261,#1261,#1091,.T.);
#1487=EDGE_CURVE('',#1261,#1262,#858,.T.);
#1488=EDGE_CURVE('',#1262,#1262,#1092,.T.);
#1489=EDGE_CURVE('',#1263,#1263,#1093,.T.);
#1490=EDGE_CURVE('',#1264,#1264,#1094,.T.);
#1491=EDGE_CURVE('',#1265,#1265,#1095,.T.);
#1492=EDGE_CURVE('',#1265,#1264,#859,.T.);
#1493=EDGE_CURVE('',#1266,#1266,#1096,.T.);
#1494=EDGE_CURVE('',#1267,#1267,#1097,.T.);
#1495=EDGE_CURVE('',#1266,#1268,#860,.T.);
#1496=EDGE_CURVE('',#1268,#1268,#1098,.T.);
#1497=EDGE_CURVE('',#1263,#1267,#861,.T.);
#1498=EDGE_CURVE('',#1269,#1269,#1099,.T.);
#1499=EDGE_CURVE('',#1269,#1270,#862,.T.);
#1500=EDGE_CURVE('',#1270,#1270,#1100,.T.);
#1501=EDGE_CURVE('',#1271,#1271,#1101,.T.);
#1502=EDGE_CURVE('',#1272,#1272,#1102,.T.);
#1503=EDGE_CURVE('',#1273,#1273,#1103,.T.);
#1504=EDGE_CURVE('',#1273,#1272,#863,.T.);
#1505=EDGE_CURVE('',#1274,#1274,#1104,.T.);
#1506=EDGE_CURVE('',#1275,#1275,#1105,.T.);
#1507=EDGE_CURVE('',#1274,#1276,#864,.T.);
#1508=EDGE_CURVE('',#1276,#1276,#1106,.T.);
#1509=EDGE_CURVE('',#1271,#1275,#865,.T.);
#1510=EDGE_CURVE('',#1277,#1277,#1107,.T.);
#1511=EDGE_CURVE('',#1277,#1278,#866,.T.);
#1512=EDGE_CURVE('',#1278,#1278,#1108,.T.);
#1513=EDGE_CURVE('',#1279,#1279,#1109,.T.);
#1514=EDGE_CURVE('',#1280,#1280,#1110,.T.);
#1515=EDGE_CURVE('',#1281,#1281,#1111,.T.);
#1516=EDGE_CURVE('',#1281,#1280,#867,.T.);
#1517=EDGE_CURVE('',#1282,#1282,#1112,.T.);
#1518=EDGE_CURVE('',#1283,#1283,#1113,.T.);
#1519=EDGE_CURVE('',#1282,#1284,#868,.T.);
#1520=EDGE_CURVE('',#1284,#1284,#1114,.T.);
#1521=EDGE_CURVE('',#1279,#1283,#869,.T.);
#1522=EDGE_CURVE('',#1285,#1285,#1115,.T.);
#1523=EDGE_CURVE('',#1286,#1286,#1116,.T.);
#1524=EDGE_CURVE('',#1287,#1287,#1117,.T.);
#1525=EDGE_CURVE('',#1288,#1288,#1118,.T.);
#1526=EDGE_CURVE('',#1285,#1287,#870,.T.);
#1527=EDGE_CURVE('',#1288,#1289,#871,.T.);
#1528=EDGE_CURVE('',#1289,#1289,#1119,.T.);
#1529=EDGE_CURVE('',#1290,#1290,#1120,.T.);
#1530=EDGE_CURVE('',#1290,#1291,#872,.T.);
#1531=EDGE_CURVE('',#1291,#1291,#1121,.T.);
#1532=EDGE_CURVE('',#1292,#1292,#1122,.T.);
#1533=EDGE_CURVE('',#1293,#1293,#1123,.T.);
#1534=EDGE_CURVE('',#1294,#1294,#1124,.T.);
#1535=EDGE_CURVE('',#1294,#1293,#873,.T.);
#1536=EDGE_CURVE('',#1295,#1295,#1125,.T.);
#1537=EDGE_CURVE('',#1295,#1296,#874,.T.);
#1538=EDGE_CURVE('',#1296,#1296,#1126,.T.);
#1539=EDGE_CURVE('',#1292,#1286,#875,.T.);
#1540=EDGE_CURVE('',#1297,#1297,#1127,.T.);
#1541=EDGE_CURVE('',#1297,#1298,#876,.T.);
#1542=EDGE_CURVE('',#1298,#1298,#1128,.T.);
#1543=EDGE_CURVE('',#1299,#1299,#1129,.T.);
#1544=EDGE_CURVE('',#1300,#1300,#1130,.T.);
#1545=EDGE_CURVE('',#1301,#1301,#1131,.T.);
#1546=EDGE_CURVE('',#1301,#1300,#877,.T.);
#1547=EDGE_CURVE('',#1302,#1302,#1132,.T.);
#1548=EDGE_CURVE('',#1303,#1303,#1133,.T.);
#1549=EDGE_CURVE('',#1302,#1304,#878,.T.);
#1550=EDGE_CURVE('',#1304,#1304,#1134,.T.);
#1551=EDGE_CURVE('',#1299,#1303,#879,.T.);
#1552=EDGE_CURVE('',#1305,#1305,#1135,.T.);
#1553=EDGE_CURVE('',#1305,#1306,#880,.T.);
#1554=EDGE_CURVE('',#1306,#1306,#1136,.T.);
#1555=EDGE_CURVE('',#1307,#1307,#1137,.T.);
#1556=EDGE_CURVE('',#1308,#1308,#1138,.T.);
#1557=EDGE_CURVE('',#1309,#1309,#1139,.T.);
#1558=EDGE_CURVE('',#1309,#1308,#881,.T.);
#1559=EDGE_CURVE('',#1310,#1310,#1140,.T.);
#1560=EDGE_CURVE('',#1311,#1311,#1141,.T.);
#1561=EDGE_CURVE('',#1310,#1312,#882,.T.);
#1562=EDGE_CURVE('',#1312,#1312,#1142,.T.);
#1563=EDGE_CURVE('',#1307,#1311,#883,.T.);
#1564=EDGE_CURVE('',#1313,#1313,#1143,.T.);
#1565=EDGE_CURVE('',#1313,#1314,#884,.T.);
#1566=EDGE_CURVE('',#1314,#1314,#1144,.T.);
#1567=EDGE_CURVE('',#1315,#1315,#1145,.T.);
#1568=EDGE_CURVE('',#1315,#1316,#885,.T.);
#1569=EDGE_CURVE('',#1316,#1316,#1146,.T.);
#1570=EDGE_CURVE('',#1317,#1317,#1147,.T.);
#1571=EDGE_CURVE('',#1317,#1318,#886,.T.);
#1572=EDGE_CURVE('',#1318,#1318,#1148,.T.);
#1573=EDGE_CURVE('',#1319,#1319,#1149,.T.);
#1574=EDGE_CURVE('',#1319,#1320,#887,.T.);
#1575=EDGE_CURVE('',#1320,#1320,#1150,.T.);
#1576=EDGE_CURVE('',#1321,#1321,#1151,.T.);
#1577=EDGE_CURVE('',#1321,#1322,#888,.T.);
#1578=EDGE_CURVE('',#1322,#1322,#1152,.T.);
#1579=EDGE_CURVE('',#1323,#1323,#1153,.T.);
#1580=EDGE_CURVE('',#1323,#1324,#889,.T.);
#1581=EDGE_CURVE('',#1324,#1324,#1154,.T.);
#1582=EDGE_CURVE('',#1325,#1326,#890,.T.);
#1583=EDGE_CURVE('',#1327,#1325,#891,.T.);
#1584=EDGE_CURVE('',#1328,#1327,#892,.T.);
#1585=EDGE_CURVE('',#1326,#1328,#893,.T.);
#1586=EDGE_CURVE('',#1329,#1330,#894,.T.);
#1587=EDGE_CURVE('',#1331,#1329,#895,.T.);
#1588=EDGE_CURVE('',#1332,#1331,#896,.T.);
#1589=EDGE_CURVE('',#1330,#1332,#897,.T.);
#1590=EDGE_CURVE('',#1327,#1332,#1155,.T.);
#1591=EDGE_CURVE('',#1330,#1325,#1156,.T.);
#1592=EDGE_CURVE('',#1329,#1326,#1157,.T.);
#1593=EDGE_CURVE('',#1328,#1331,#1158,.T.);
#1594=ORIENTED_EDGE('',*,*,#1333,.F.);
#1595=ORIENTED_EDGE('',*,*,#1334,.T.);
#1596=ORIENTED_EDGE('',*,*,#1335,.F.);
#1597=ORIENTED_EDGE('',*,*,#1334,.F.);
#1598=ORIENTED_EDGE('',*,*,#1336,.F.);
#1599=ORIENTED_EDGE('',*,*,#1337,.T.);
#1600=ORIENTED_EDGE('',*,*,#1338,.F.);
#1601=ORIENTED_EDGE('',*,*,#1337,.F.);
#1602=ORIENTED_EDGE('',*,*,#1339,.T.);
#1603=ORIENTED_EDGE('',*,*,#1340,.T.);
#1604=ORIENTED_EDGE('',*,*,#1341,.F.);
#1605=ORIENTED_EDGE('',*,*,#1342,.F.);
#1606=ORIENTED_EDGE('',*,*,#1343,.T.);
#1607=ORIENTED_EDGE('',*,*,#1342,.T.);
#1608=ORIENTED_EDGE('',*,*,#1344,.F.);
#1609=ORIENTED_EDGE('',*,*,#1345,.F.);
#1610=ORIENTED_EDGE('',*,*,#1346,.T.);
#1611=ORIENTED_EDGE('',*,*,#1345,.T.);
#1612=ORIENTED_EDGE('',*,*,#1347,.F.);
#1613=ORIENTED_EDGE('',*,*,#1348,.F.);
#1614=ORIENTED_EDGE('',*,*,#1349,.T.);
#1615=ORIENTED_EDGE('',*,*,#1348,.T.);
#1616=ORIENTED_EDGE('',*,*,#1350,.F.);
#1617=ORIENTED_EDGE('',*,*,#1340,.F.);
#1618=ORIENTED_EDGE('',*,*,#1350,.T.);
#1619=ORIENTED_EDGE('',*,*,#1347,.T.);
#1620=ORIENTED_EDGE('',*,*,#1344,.T.);
#1621=ORIENTED_EDGE('',*,*,#1341,.T.);
#1622=ORIENTED_EDGE('',*,*,#1333,.T.);
#1623=ORIENTED_EDGE('',*,*,#1336,.T.);
#1624=ORIENTED_EDGE('',*,*,#1349,.F.);
#1625=ORIENTED_EDGE('',*,*,#1339,.F.);
#1626=ORIENTED_EDGE('',*,*,#1343,.F.);
#1627=ORIENTED_EDGE('',*,*,#1346,.F.);
#1628=ORIENTED_EDGE('',*,*,#1335,.T.);
#1629=ORIENTED_EDGE('',*,*,#1338,.T.);
#1630=ORIENTED_EDGE('',*,*,#1351,.F.);
#1631=ORIENTED_EDGE('',*,*,#1352,.T.);
#1632=ORIENTED_EDGE('',*,*,#1353,.T.);
#1633=ORIENTED_EDGE('',*,*,#1352,.F.);
#1634=ORIENTED_EDGE('',*,*,#1354,.F.);
#1635=ORIENTED_EDGE('',*,*,#1355,.T.);
#1636=ORIENTED_EDGE('',*,*,#1356,.T.);
#1637=ORIENTED_EDGE('',*,*,#1355,.F.);
#1638=ORIENTED_EDGE('',*,*,#1354,.T.);
#1639=ORIENTED_EDGE('',*,*,#1351,.T.);
#1640=ORIENTED_EDGE('',*,*,#1356,.F.);
#1641=ORIENTED_EDGE('',*,*,#1353,.F.);
#1642=ORIENTED_EDGE('',*,*,#1357,.F.);
#1643=ORIENTED_EDGE('',*,*,#1358,.T.);
#1644=ORIENTED_EDGE('',*,*,#1359,.T.);
#1645=ORIENTED_EDGE('',*,*,#1358,.F.);
#1646=ORIENTED_EDGE('',*,*,#1360,.F.);
#1647=ORIENTED_EDGE('',*,*,#1361,.T.);
#1648=ORIENTED_EDGE('',*,*,#1362,.T.);
#1649=ORIENTED_EDGE('',*,*,#1361,.F.);
#1650=ORIENTED_EDGE('',*,*,#1360,.T.);
#1651=ORIENTED_EDGE('',*,*,#1357,.T.);
#1652=ORIENTED_EDGE('',*,*,#1362,.F.);
#1653=ORIENTED_EDGE('',*,*,#1359,.F.);
#1654=ORIENTED_EDGE('',*,*,#1363,.F.);
#1655=ORIENTED_EDGE('',*,*,#1364,.T.);
#1656=ORIENTED_EDGE('',*,*,#1365,.F.);
#1657=ORIENTED_EDGE('',*,*,#1364,.F.);
#1658=ORIENTED_EDGE('',*,*,#1366,.F.);
#1659=ORIENTED_EDGE('',*,*,#1367,.T.);
#1660=ORIENTED_EDGE('',*,*,#1368,.F.);
#1661=ORIENTED_EDGE('',*,*,#1367,.F.);
#1662=ORIENTED_EDGE('',*,*,#1369,.T.);
#1663=ORIENTED_EDGE('',*,*,#1370,.T.);
#1664=ORIENTED_EDGE('',*,*,#1371,.F.);
#1665=ORIENTED_EDGE('',*,*,#1372,.F.);
#1666=ORIENTED_EDGE('',*,*,#1373,.T.);
#1667=ORIENTED_EDGE('',*,*,#1372,.T.);
#1668=ORIENTED_EDGE('',*,*,#1374,.F.);
#1669=ORIENTED_EDGE('',*,*,#1375,.F.);
#1670=ORIENTED_EDGE('',*,*,#1376,.T.);
#1671=ORIENTED_EDGE('',*,*,#1375,.T.);
#1672=ORIENTED_EDGE('',*,*,#1377,.F.);
#1673=ORIENTED_EDGE('',*,*,#1378,.F.);
#1674=ORIENTED_EDGE('',*,*,#1379,.T.);
#1675=ORIENTED_EDGE('',*,*,#1378,.T.);
#1676=ORIENTED_EDGE('',*,*,#1380,.F.);
#1677=ORIENTED_EDGE('',*,*,#1370,.F.);
#1678=ORIENTED_EDGE('',*,*,#1380,.T.);
#1679=ORIENTED_EDGE('',*,*,#1377,.T.);
#1680=ORIENTED_EDGE('',*,*,#1374,.T.);
#1681=ORIENTED_EDGE('',*,*,#1371,.T.);
#1682=ORIENTED_EDGE('',*,*,#1363,.T.);
#1683=ORIENTED_EDGE('',*,*,#1366,.T.);
#1684=ORIENTED_EDGE('',*,*,#1379,.F.);
#1685=ORIENTED_EDGE('',*,*,#1369,.F.);
#1686=ORIENTED_EDGE('',*,*,#1373,.F.);
#1687=ORIENTED_EDGE('',*,*,#1376,.F.);
#1688=ORIENTED_EDGE('',*,*,#1365,.T.);
#1689=ORIENTED_EDGE('',*,*,#1368,.T.);
#1690=ORIENTED_EDGE('',*,*,#1381,.F.);
#1691=ORIENTED_EDGE('',*,*,#1382,.T.);
#1692=ORIENTED_EDGE('',*,*,#1383,.F.);
#1693=ORIENTED_EDGE('',*,*,#1384,.F.);
#1694=ORIENTED_EDGE('',*,*,#1385,.F.);
#1695=ORIENTED_EDGE('',*,*,#1386,.T.);
#1696=ORIENTED_EDGE('',*,*,#1387,.F.);
#1697=ORIENTED_EDGE('',*,*,#1382,.F.);
#1698=ORIENTED_EDGE('',*,*,#1388,.F.);
#1699=ORIENTED_EDGE('',*,*,#1389,.T.);
#1700=ORIENTED_EDGE('',*,*,#1390,.F.);
#1701=ORIENTED_EDGE('',*,*,#1386,.F.);
#1702=ORIENTED_EDGE('',*,*,#1391,.F.);
#1703=ORIENTED_EDGE('',*,*,#1384,.T.);
#1704=ORIENTED_EDGE('',*,*,#1392,.F.);
#1705=ORIENTED_EDGE('',*,*,#1389,.F.);
#1706=ORIENTED_EDGE('',*,*,#1393,.F.);
#1707=ORIENTED_EDGE('',*,*,#1394,.T.);
#1708=ORIENTED_EDGE('',*,*,#1395,.F.);
#1709=ORIENTED_EDGE('',*,*,#1394,.F.);
#1710=ORIENTED_EDGE('',*,*,#1396,.F.);
#1711=ORIENTED_EDGE('',*,*,#1397,.T.);
#1712=ORIENTED_EDGE('',*,*,#1398,.F.);
#1713=ORIENTED_EDGE('',*,*,#1397,.F.);
#1714=ORIENTED_EDGE('',*,*,#1399,.T.);
#1715=ORIENTED_EDGE('',*,*,#1400,.T.);
#1716=ORIENTED_EDGE('',*,*,#1401,.F.);
#1717=ORIENTED_EDGE('',*,*,#1402,.F.);
#1718=ORIENTED_EDGE('',*,*,#1403,.T.);
#1719=ORIENTED_EDGE('',*,*,#1402,.T.);
#1720=ORIENTED_EDGE('',*,*,#1404,.F.);
#1721=ORIENTED_EDGE('',*,*,#1405,.F.);
#1722=ORIENTED_EDGE('',*,*,#1406,.T.);
#1723=ORIENTED_EDGE('',*,*,#1405,.T.);
#1724=ORIENTED_EDGE('',*,*,#1407,.F.);
#1725=ORIENTED_EDGE('',*,*,#1408,.F.);
#1726=ORIENTED_EDGE('',*,*,#1409,.T.);
#1727=ORIENTED_EDGE('',*,*,#1408,.T.);
#1728=ORIENTED_EDGE('',*,*,#1410,.F.);
#1729=ORIENTED_EDGE('',*,*,#1400,.F.);
#1730=ORIENTED_EDGE('',*,*,#1410,.T.);
#1731=ORIENTED_EDGE('',*,*,#1407,.T.);
#1732=ORIENTED_EDGE('',*,*,#1404,.T.);
#1733=ORIENTED_EDGE('',*,*,#1401,.T.);
#1734=ORIENTED_EDGE('',*,*,#1381,.T.);
#1735=ORIENTED_EDGE('',*,*,#1391,.T.);
#1736=ORIENTED_EDGE('',*,*,#1388,.T.);
#1737=ORIENTED_EDGE('',*,*,#1385,.T.);
#1738=ORIENTED_EDGE('',*,*,#1393,.T.);
#1739=ORIENTED_EDGE('',*,*,#1396,.T.);
#1740=ORIENTED_EDGE('',*,*,#1409,.F.);
#1741=ORIENTED_EDGE('',*,*,#1399,.F.);
#1742=ORIENTED_EDGE('',*,*,#1403,.F.);
#1743=ORIENTED_EDGE('',*,*,#1406,.F.);
#1744=ORIENTED_EDGE('',*,*,#1383,.T.);
#1745=ORIENTED_EDGE('',*,*,#1387,.T.);
#1746=ORIENTED_EDGE('',*,*,#1390,.T.);
#1747=ORIENTED_EDGE('',*,*,#1392,.T.);
#1748=ORIENTED_EDGE('',*,*,#1395,.T.);
#1749=ORIENTED_EDGE('',*,*,#1398,.T.);
#1750=ORIENTED_EDGE('',*,*,#1411,.F.);
#1751=ORIENTED_EDGE('',*,*,#1412,.T.);
#1752=ORIENTED_EDGE('',*,*,#1413,.F.);
#1753=ORIENTED_EDGE('',*,*,#1412,.F.);
#1754=ORIENTED_EDGE('',*,*,#1414,.F.);
#1755=ORIENTED_EDGE('',*,*,#1415,.T.);
#1756=ORIENTED_EDGE('',*,*,#1416,.F.);
#1757=ORIENTED_EDGE('',*,*,#1415,.F.);
#1758=ORIENTED_EDGE('',*,*,#1417,.T.);
#1759=ORIENTED_EDGE('',*,*,#1418,.T.);
#1760=ORIENTED_EDGE('',*,*,#1419,.F.);
#1761=ORIENTED_EDGE('',*,*,#1420,.F.);
#1762=ORIENTED_EDGE('',*,*,#1421,.T.);
#1763=ORIENTED_EDGE('',*,*,#1420,.T.);
#1764=ORIENTED_EDGE('',*,*,#1422,.F.);
#1765=ORIENTED_EDGE('',*,*,#1423,.F.);
#1766=ORIENTED_EDGE('',*,*,#1424,.T.);
#1767=ORIENTED_EDGE('',*,*,#1423,.T.);
#1768=ORIENTED_EDGE('',*,*,#1425,.F.);
#1769=ORIENTED_EDGE('',*,*,#1426,.F.);
#1770=ORIENTED_EDGE('',*,*,#1427,.T.);
#1771=ORIENTED_EDGE('',*,*,#1426,.T.);
#1772=ORIENTED_EDGE('',*,*,#1428,.F.);
#1773=ORIENTED_EDGE('',*,*,#1418,.F.);
#1774=ORIENTED_EDGE('',*,*,#1428,.T.);
#1775=ORIENTED_EDGE('',*,*,#1425,.T.);
#1776=ORIENTED_EDGE('',*,*,#1422,.T.);
#1777=ORIENTED_EDGE('',*,*,#1419,.T.);
#1778=ORIENTED_EDGE('',*,*,#1411,.T.);
#1779=ORIENTED_EDGE('',*,*,#1414,.T.);
#1780=ORIENTED_EDGE('',*,*,#1427,.F.);
#1781=ORIENTED_EDGE('',*,*,#1417,.F.);
#1782=ORIENTED_EDGE('',*,*,#1421,.F.);
#1783=ORIENTED_EDGE('',*,*,#1424,.F.);
#1784=ORIENTED_EDGE('',*,*,#1413,.T.);
#1785=ORIENTED_EDGE('',*,*,#1416,.T.);
#1786=ORIENTED_EDGE('',*,*,#1429,.F.);
#1787=ORIENTED_EDGE('',*,*,#1430,.T.);
#1788=ORIENTED_EDGE('',*,*,#1431,.F.);
#1789=ORIENTED_EDGE('',*,*,#1430,.F.);
#1790=ORIENTED_EDGE('',*,*,#1432,.T.);
#1791=ORIENTED_EDGE('',*,*,#1433,.T.);
#1792=ORIENTED_EDGE('',*,*,#1434,.F.);
#1793=ORIENTED_EDGE('',*,*,#1435,.F.);
#1794=ORIENTED_EDGE('',*,*,#1436,.T.);
#1795=ORIENTED_EDGE('',*,*,#1435,.T.);
#1796=ORIENTED_EDGE('',*,*,#1437,.F.);
#1797=ORIENTED_EDGE('',*,*,#1438,.F.);
#1798=ORIENTED_EDGE('',*,*,#1439,.T.);
#1799=ORIENTED_EDGE('',*,*,#1438,.T.);
#1800=ORIENTED_EDGE('',*,*,#1440,.F.);
#1801=ORIENTED_EDGE('',*,*,#1441,.F.);
#1802=ORIENTED_EDGE('',*,*,#1442,.T.);
#1803=ORIENTED_EDGE('',*,*,#1441,.T.);
#1804=ORIENTED_EDGE('',*,*,#1443,.F.);
#1805=ORIENTED_EDGE('',*,*,#1433,.F.);
#1806=ORIENTED_EDGE('',*,*,#1443,.T.);
#1807=ORIENTED_EDGE('',*,*,#1440,.T.);
#1808=ORIENTED_EDGE('',*,*,#1437,.T.);
#1809=ORIENTED_EDGE('',*,*,#1434,.T.);
#1810=ORIENTED_EDGE('',*,*,#1429,.T.);
#1811=ORIENTED_EDGE('',*,*,#1442,.F.);
#1812=ORIENTED_EDGE('',*,*,#1432,.F.);
#1813=ORIENTED_EDGE('',*,*,#1436,.F.);
#1814=ORIENTED_EDGE('',*,*,#1439,.F.);
#1815=ORIENTED_EDGE('',*,*,#1431,.T.);
#1816=ORIENTED_EDGE('',*,*,#1444,.F.);
#1817=ORIENTED_EDGE('',*,*,#1445,.T.);
#1818=ORIENTED_EDGE('',*,*,#1446,.F.);
#1819=ORIENTED_EDGE('',*,*,#1445,.F.);
#1820=ORIENTED_EDGE('',*,*,#1447,.F.);
#1821=ORIENTED_EDGE('',*,*,#1448,.T.);
#1822=ORIENTED_EDGE('',*,*,#1449,.F.);
#1823=ORIENTED_EDGE('',*,*,#1448,.F.);
#1824=ORIENTED_EDGE('',*,*,#1450,.F.);
#1825=ORIENTED_EDGE('',*,*,#1451,.T.);
#1826=ORIENTED_EDGE('',*,*,#1452,.F.);
#1827=ORIENTED_EDGE('',*,*,#1451,.F.);
#1828=ORIENTED_EDGE('',*,*,#1453,.T.);
#1829=ORIENTED_EDGE('',*,*,#1454,.T.);
#1830=ORIENTED_EDGE('',*,*,#1455,.F.);
#1831=ORIENTED_EDGE('',*,*,#1456,.F.);
#1832=ORIENTED_EDGE('',*,*,#1447,.T.);
#1833=ORIENTED_EDGE('',*,*,#1450,.T.);
#1834=ORIENTED_EDGE('',*,*,#1457,.T.);
#1835=ORIENTED_EDGE('',*,*,#1456,.T.);
#1836=ORIENTED_EDGE('',*,*,#1458,.F.);
#1837=ORIENTED_EDGE('',*,*,#1459,.F.);
#1838=ORIENTED_EDGE('',*,*,#1460,.T.);
#1839=ORIENTED_EDGE('',*,*,#1459,.T.);
#1840=ORIENTED_EDGE('',*,*,#1461,.F.);
#1841=ORIENTED_EDGE('',*,*,#1462,.F.);
#1842=ORIENTED_EDGE('',*,*,#1449,.T.);
#1843=ORIENTED_EDGE('',*,*,#1452,.T.);
#1844=ORIENTED_EDGE('',*,*,#1463,.T.);
#1845=ORIENTED_EDGE('',*,*,#1462,.T.);
#1846=ORIENTED_EDGE('',*,*,#1464,.F.);
#1847=ORIENTED_EDGE('',*,*,#1454,.F.);
#1848=ORIENTED_EDGE('',*,*,#1464,.T.);
#1849=ORIENTED_EDGE('',*,*,#1461,.T.);
#1850=ORIENTED_EDGE('',*,*,#1458,.T.);
#1851=ORIENTED_EDGE('',*,*,#1455,.T.);
#1852=ORIENTED_EDGE('',*,*,#1444,.T.);
#1853=ORIENTED_EDGE('',*,*,#1463,.F.);
#1854=ORIENTED_EDGE('',*,*,#1453,.F.);
#1855=ORIENTED_EDGE('',*,*,#1457,.F.);
#1856=ORIENTED_EDGE('',*,*,#1460,.F.);
#1857=ORIENTED_EDGE('',*,*,#1446,.T.);
#1858=ORIENTED_EDGE('',*,*,#1465,.F.);
#1859=ORIENTED_EDGE('',*,*,#1466,.T.);
#1860=ORIENTED_EDGE('',*,*,#1467,.T.);
#1861=ORIENTED_EDGE('',*,*,#1466,.F.);
#1862=ORIENTED_EDGE('',*,*,#1468,.F.);
#1863=ORIENTED_EDGE('',*,*,#1469,.T.);
#1864=ORIENTED_EDGE('',*,*,#1470,.T.);
#1865=ORIENTED_EDGE('',*,*,#1469,.F.);
#1866=ORIENTED_EDGE('',*,*,#1468,.T.);
#1867=ORIENTED_EDGE('',*,*,#1465,.T.);
#1868=ORIENTED_EDGE('',*,*,#1470,.F.);
#1869=ORIENTED_EDGE('',*,*,#1467,.F.);
#1870=ORIENTED_EDGE('',*,*,#1471,.F.);
#1871=ORIENTED_EDGE('',*,*,#1472,.T.);
#1872=ORIENTED_EDGE('',*,*,#1473,.F.);
#1873=ORIENTED_EDGE('',*,*,#1472,.F.);
#1874=ORIENTED_EDGE('',*,*,#1474,.T.);
#1875=ORIENTED_EDGE('',*,*,#1475,.T.);
#1876=ORIENTED_EDGE('',*,*,#1476,.F.);
#1877=ORIENTED_EDGE('',*,*,#1477,.F.);
#1878=ORIENTED_EDGE('',*,*,#1471,.T.);
#1879=ORIENTED_EDGE('',*,*,#1478,.T.);
#1880=ORIENTED_EDGE('',*,*,#1477,.T.);
#1881=ORIENTED_EDGE('',*,*,#1479,.F.);
#1882=ORIENTED_EDGE('',*,*,#1480,.F.);
#1883=ORIENTED_EDGE('',*,*,#1481,.T.);
#1884=ORIENTED_EDGE('',*,*,#1480,.T.);
#1885=ORIENTED_EDGE('',*,*,#1482,.F.);
#1886=ORIENTED_EDGE('',*,*,#1483,.F.);
#1887=ORIENTED_EDGE('',*,*,#1473,.T.);
#1888=ORIENTED_EDGE('',*,*,#1484,.T.);
#1889=ORIENTED_EDGE('',*,*,#1483,.T.);
#1890=ORIENTED_EDGE('',*,*,#1485,.F.);
#1891=ORIENTED_EDGE('',*,*,#1475,.F.);
#1892=ORIENTED_EDGE('',*,*,#1485,.T.);
#1893=ORIENTED_EDGE('',*,*,#1482,.T.);
#1894=ORIENTED_EDGE('',*,*,#1479,.T.);
#1895=ORIENTED_EDGE('',*,*,#1476,.T.);
#1896=ORIENTED_EDGE('',*,*,#1484,.F.);
#1897=ORIENTED_EDGE('',*,*,#1474,.F.);
#1898=ORIENTED_EDGE('',*,*,#1478,.F.);
#1899=ORIENTED_EDGE('',*,*,#1481,.F.);
#1900=ORIENTED_EDGE('',*,*,#1486,.T.);
#1901=ORIENTED_EDGE('',*,*,#1487,.T.);
#1902=ORIENTED_EDGE('',*,*,#1488,.F.);
#1903=ORIENTED_EDGE('',*,*,#1487,.F.);
#1904=ORIENTED_EDGE('',*,*,#1489,.F.);
#1905=ORIENTED_EDGE('',*,*,#1486,.F.);
#1906=ORIENTED_EDGE('',*,*,#1490,.F.);
#1907=ORIENTED_EDGE('',*,*,#1488,.T.);
#1908=ORIENTED_EDGE('',*,*,#1491,.F.);
#1909=ORIENTED_EDGE('',*,*,#1492,.T.);
#1910=ORIENTED_EDGE('',*,*,#1490,.T.);
#1911=ORIENTED_EDGE('',*,*,#1492,.F.);
#1912=ORIENTED_EDGE('',*,*,#1493,.T.);
#1913=ORIENTED_EDGE('',*,*,#1494,.F.);
#1914=ORIENTED_EDGE('',*,*,#1493,.F.);
#1915=ORIENTED_EDGE('',*,*,#1495,.T.);
#1916=ORIENTED_EDGE('',*,*,#1496,.T.);
#1917=ORIENTED_EDGE('',*,*,#1495,.F.);
#1918=ORIENTED_EDGE('',*,*,#1496,.F.);
#1919=ORIENTED_EDGE('',*,*,#1489,.T.);
#1920=ORIENTED_EDGE('',*,*,#1497,.T.);
#1921=ORIENTED_EDGE('',*,*,#1494,.T.);
#1922=ORIENTED_EDGE('',*,*,#1497,.F.);
#1923=ORIENTED_EDGE('',*,*,#1491,.T.);
#1924=ORIENTED_EDGE('',*,*,#1498,.T.);
#1925=ORIENTED_EDGE('',*,*,#1499,.T.);
#1926=ORIENTED_EDGE('',*,*,#1500,.F.);
#1927=ORIENTED_EDGE('',*,*,#1499,.F.);
#1928=ORIENTED_EDGE('',*,*,#1501,.F.);
#1929=ORIENTED_EDGE('',*,*,#1498,.F.);
#1930=ORIENTED_EDGE('',*,*,#1502,.F.);
#1931=ORIENTED_EDGE('',*,*,#1500,.T.);
#1932=ORIENTED_EDGE('',*,*,#1503,.F.);
#1933=ORIENTED_EDGE('',*,*,#1504,.T.);
#1934=ORIENTED_EDGE('',*,*,#1502,.T.);
#1935=ORIENTED_EDGE('',*,*,#1504,.F.);
#1936=ORIENTED_EDGE('',*,*,#1505,.T.);
#1937=ORIENTED_EDGE('',*,*,#1506,.F.);
#1938=ORIENTED_EDGE('',*,*,#1505,.F.);
#1939=ORIENTED_EDGE('',*,*,#1507,.T.);
#1940=ORIENTED_EDGE('',*,*,#1508,.T.);
#1941=ORIENTED_EDGE('',*,*,#1507,.F.);
#1942=ORIENTED_EDGE('',*,*,#1508,.F.);
#1943=ORIENTED_EDGE('',*,*,#1501,.T.);
#1944=ORIENTED_EDGE('',*,*,#1509,.T.);
#1945=ORIENTED_EDGE('',*,*,#1506,.T.);
#1946=ORIENTED_EDGE('',*,*,#1509,.F.);
#1947=ORIENTED_EDGE('',*,*,#1503,.T.);
#1948=ORIENTED_EDGE('',*,*,#1510,.T.);
#1949=ORIENTED_EDGE('',*,*,#1511,.T.);
#1950=ORIENTED_EDGE('',*,*,#1512,.F.);
#1951=ORIENTED_EDGE('',*,*,#1511,.F.);
#1952=ORIENTED_EDGE('',*,*,#1513,.F.);
#1953=ORIENTED_EDGE('',*,*,#1510,.F.);
#1954=ORIENTED_EDGE('',*,*,#1514,.F.);
#1955=ORIENTED_EDGE('',*,*,#1512,.T.);
#1956=ORIENTED_EDGE('',*,*,#1515,.F.);
#1957=ORIENTED_EDGE('',*,*,#1516,.T.);
#1958=ORIENTED_EDGE('',*,*,#1514,.T.);
#1959=ORIENTED_EDGE('',*,*,#1516,.F.);
#1960=ORIENTED_EDGE('',*,*,#1517,.T.);
#1961=ORIENTED_EDGE('',*,*,#1518,.F.);
#1962=ORIENTED_EDGE('',*,*,#1517,.F.);
#1963=ORIENTED_EDGE('',*,*,#1519,.T.);
#1964=ORIENTED_EDGE('',*,*,#1520,.T.);
#1965=ORIENTED_EDGE('',*,*,#1519,.F.);
#1966=ORIENTED_EDGE('',*,*,#1520,.F.);
#1967=ORIENTED_EDGE('',*,*,#1513,.T.);
#1968=ORIENTED_EDGE('',*,*,#1521,.T.);
#1969=ORIENTED_EDGE('',*,*,#1518,.T.);
#1970=ORIENTED_EDGE('',*,*,#1521,.F.);
#1971=ORIENTED_EDGE('',*,*,#1515,.T.);
#1972=ORIENTED_EDGE('',*,*,#1522,.T.);
#1973=ORIENTED_EDGE('',*,*,#1523,.F.);
#1974=ORIENTED_EDGE('',*,*,#1524,.F.);
#1975=ORIENTED_EDGE('',*,*,#1525,.F.);
#1976=ORIENTED_EDGE('',*,*,#1522,.F.);
#1977=ORIENTED_EDGE('',*,*,#1526,.T.);
#1978=ORIENTED_EDGE('',*,*,#1524,.T.);
#1979=ORIENTED_EDGE('',*,*,#1526,.F.);
#1980=ORIENTED_EDGE('',*,*,#1525,.T.);
#1981=ORIENTED_EDGE('',*,*,#1527,.T.);
#1982=ORIENTED_EDGE('',*,*,#1528,.T.);
#1983=ORIENTED_EDGE('',*,*,#1527,.F.);
#1984=ORIENTED_EDGE('',*,*,#1529,.T.);
#1985=ORIENTED_EDGE('',*,*,#1530,.T.);
#1986=ORIENTED_EDGE('',*,*,#1531,.F.);
#1987=ORIENTED_EDGE('',*,*,#1530,.F.);
#1988=ORIENTED_EDGE('',*,*,#1532,.F.);
#1989=ORIENTED_EDGE('',*,*,#1529,.F.);
#1990=ORIENTED_EDGE('',*,*,#1533,.F.);
#1991=ORIENTED_EDGE('',*,*,#1531,.T.);
#1992=ORIENTED_EDGE('',*,*,#1534,.F.);
#1993=ORIENTED_EDGE('',*,*,#1535,.T.);
#1994=ORIENTED_EDGE('',*,*,#1533,.T.);
#1995=ORIENTED_EDGE('',*,*,#1535,.F.);
#1996=ORIENTED_EDGE('',*,*,#1536,.T.);
#1997=ORIENTED_EDGE('',*,*,#1528,.F.);
#1998=ORIENTED_EDGE('',*,*,#1536,.F.);
#1999=ORIENTED_EDGE('',*,*,#1537,.T.);
#2000=ORIENTED_EDGE('',*,*,#1538,.T.);
#2001=ORIENTED_EDGE('',*,*,#1537,.F.);
#2002=ORIENTED_EDGE('',*,*,#1538,.F.);
#2003=ORIENTED_EDGE('',*,*,#1532,.T.);
#2004=ORIENTED_EDGE('',*,*,#1539,.T.);
#2005=ORIENTED_EDGE('',*,*,#1523,.T.);
#2006=ORIENTED_EDGE('',*,*,#1539,.F.);
#2007=ORIENTED_EDGE('',*,*,#1534,.T.);
#2008=ORIENTED_EDGE('',*,*,#1540,.T.);
#2009=ORIENTED_EDGE('',*,*,#1541,.T.);
#2010=ORIENTED_EDGE('',*,*,#1542,.F.);
#2011=ORIENTED_EDGE('',*,*,#1541,.F.);
#2012=ORIENTED_EDGE('',*,*,#1543,.F.);
#2013=ORIENTED_EDGE('',*,*,#1540,.F.);
#2014=ORIENTED_EDGE('',*,*,#1544,.F.);
#2015=ORIENTED_EDGE('',*,*,#1542,.T.);
#2016=ORIENTED_EDGE('',*,*,#1545,.F.);
#2017=ORIENTED_EDGE('',*,*,#1546,.T.);
#2018=ORIENTED_EDGE('',*,*,#1544,.T.);
#2019=ORIENTED_EDGE('',*,*,#1546,.F.);
#2020=ORIENTED_EDGE('',*,*,#1547,.T.);
#2021=ORIENTED_EDGE('',*,*,#1548,.F.);
#2022=ORIENTED_EDGE('',*,*,#1547,.F.);
#2023=ORIENTED_EDGE('',*,*,#1549,.T.);
#2024=ORIENTED_EDGE('',*,*,#1550,.T.);
#2025=ORIENTED_EDGE('',*,*,#1549,.F.);
#2026=ORIENTED_EDGE('',*,*,#1550,.F.);
#2027=ORIENTED_EDGE('',*,*,#1543,.T.);
#2028=ORIENTED_EDGE('',*,*,#1551,.T.);
#2029=ORIENTED_EDGE('',*,*,#1548,.T.);
#2030=ORIENTED_EDGE('',*,*,#1551,.F.);
#2031=ORIENTED_EDGE('',*,*,#1545,.T.);
#2032=ORIENTED_EDGE('',*,*,#1552,.T.);
#2033=ORIENTED_EDGE('',*,*,#1553,.T.);
#2034=ORIENTED_EDGE('',*,*,#1554,.F.);
#2035=ORIENTED_EDGE('',*,*,#1553,.F.);
#2036=ORIENTED_EDGE('',*,*,#1555,.F.);
#2037=ORIENTED_EDGE('',*,*,#1552,.F.);
#2038=ORIENTED_EDGE('',*,*,#1556,.F.);
#2039=ORIENTED_EDGE('',*,*,#1554,.T.);
#2040=ORIENTED_EDGE('',*,*,#1557,.F.);
#2041=ORIENTED_EDGE('',*,*,#1558,.T.);
#2042=ORIENTED_EDGE('',*,*,#1556,.T.);
#2043=ORIENTED_EDGE('',*,*,#1558,.F.);
#2044=ORIENTED_EDGE('',*,*,#1559,.T.);
#2045=ORIENTED_EDGE('',*,*,#1560,.F.);
#2046=ORIENTED_EDGE('',*,*,#1559,.F.);
#2047=ORIENTED_EDGE('',*,*,#1561,.T.);
#2048=ORIENTED_EDGE('',*,*,#1562,.T.);
#2049=ORIENTED_EDGE('',*,*,#1561,.F.);
#2050=ORIENTED_EDGE('',*,*,#1562,.F.);
#2051=ORIENTED_EDGE('',*,*,#1555,.T.);
#2052=ORIENTED_EDGE('',*,*,#1563,.T.);
#2053=ORIENTED_EDGE('',*,*,#1560,.T.);
#2054=ORIENTED_EDGE('',*,*,#1563,.F.);
#2055=ORIENTED_EDGE('',*,*,#1557,.T.);
#2056=ORIENTED_EDGE('',*,*,#1564,.F.);
#2057=ORIENTED_EDGE('',*,*,#1565,.T.);
#2058=ORIENTED_EDGE('',*,*,#1566,.T.);
#2059=ORIENTED_EDGE('',*,*,#1565,.F.);
#2060=ORIENTED_EDGE('',*,*,#1567,.F.);
#2061=ORIENTED_EDGE('',*,*,#1568,.T.);
#2062=ORIENTED_EDGE('',*,*,#1569,.T.);
#2063=ORIENTED_EDGE('',*,*,#1568,.F.);
#2064=ORIENTED_EDGE('',*,*,#1567,.T.);
#2065=ORIENTED_EDGE('',*,*,#1564,.T.);
#2066=ORIENTED_EDGE('',*,*,#1569,.F.);
#2067=ORIENTED_EDGE('',*,*,#1566,.F.);
#2068=ORIENTED_EDGE('',*,*,#1570,.F.);
#2069=ORIENTED_EDGE('',*,*,#1571,.T.);
#2070=ORIENTED_EDGE('',*,*,#1572,.T.);
#2071=ORIENTED_EDGE('',*,*,#1571,.F.);
#2072=ORIENTED_EDGE('',*,*,#1573,.F.);
#2073=ORIENTED_EDGE('',*,*,#1574,.T.);
#2074=ORIENTED_EDGE('',*,*,#1575,.T.);
#2075=ORIENTED_EDGE('',*,*,#1574,.F.);
#2076=ORIENTED_EDGE('',*,*,#1573,.T.);
#2077=ORIENTED_EDGE('',*,*,#1570,.T.);
#2078=ORIENTED_EDGE('',*,*,#1575,.F.);
#2079=ORIENTED_EDGE('',*,*,#1572,.F.);
#2080=ORIENTED_EDGE('',*,*,#1576,.F.);
#2081=ORIENTED_EDGE('',*,*,#1577,.T.);
#2082=ORIENTED_EDGE('',*,*,#1578,.T.);
#2083=ORIENTED_EDGE('',*,*,#1577,.F.);
#2084=ORIENTED_EDGE('',*,*,#1579,.F.);
#2085=ORIENTED_EDGE('',*,*,#1580,.T.);
#2086=ORIENTED_EDGE('',*,*,#1581,.T.);
#2087=ORIENTED_EDGE('',*,*,#1580,.F.);
#2088=ORIENTED_EDGE('',*,*,#1579,.T.);
#2089=ORIENTED_EDGE('',*,*,#1576,.T.);
#2090=ORIENTED_EDGE('',*,*,#1581,.F.);
#2091=ORIENTED_EDGE('',*,*,#1578,.F.);
#2092=ORIENTED_EDGE('',*,*,#1582,.F.);
#2093=ORIENTED_EDGE('',*,*,#1583,.F.);
#2094=ORIENTED_EDGE('',*,*,#1584,.F.);
#2095=ORIENTED_EDGE('',*,*,#1585,.F.);
#2096=ORIENTED_EDGE('',*,*,#1586,.F.);
#2097=ORIENTED_EDGE('',*,*,#1587,.F.);
#2098=ORIENTED_EDGE('',*,*,#1588,.F.);
#2099=ORIENTED_EDGE('',*,*,#1589,.F.);
#2100=ORIENTED_EDGE('',*,*,#1589,.T.);
#2101=ORIENTED_EDGE('',*,*,#1590,.F.);
#2102=ORIENTED_EDGE('',*,*,#1583,.T.);
#2103=ORIENTED_EDGE('',*,*,#1591,.F.);
#2104=ORIENTED_EDGE('',*,*,#1586,.T.);
#2105=ORIENTED_EDGE('',*,*,#1591,.T.);
#2106=ORIENTED_EDGE('',*,*,#1582,.T.);
#2107=ORIENTED_EDGE('',*,*,#1592,.F.);
#2108=ORIENTED_EDGE('',*,*,#1588,.T.);
#2109=ORIENTED_EDGE('',*,*,#1593,.F.);
#2110=ORIENTED_EDGE('',*,*,#1584,.T.);
#2111=ORIENTED_EDGE('',*,*,#1590,.T.);
#2112=ORIENTED_EDGE('',*,*,#1587,.T.);
#2113=ORIENTED_EDGE('',*,*,#1592,.T.);
#2114=ORIENTED_EDGE('',*,*,#1585,.T.);
#2115=ORIENTED_EDGE('',*,*,#1593,.T.);
#2116=CYLINDRICAL_SURFACE('',#2567,5.);
#2117=CYLINDRICAL_SURFACE('',#2570,5.);
#2118=CYLINDRICAL_SURFACE('',#2580,5.);
#2119=CYLINDRICAL_SURFACE('',#2583,12.);
#2120=CYLINDRICAL_SURFACE('',#2589,5.);
#2121=CYLINDRICAL_SURFACE('',#2592,12.);
#2122=CYLINDRICAL_SURFACE('',#2598,7.);
#2123=CYLINDRICAL_SURFACE('',#2601,7.);
#2124=CYLINDRICAL_SURFACE('',#2605,12.);
#2125=CYLINDRICAL_SURFACE('',#2609,12.);
#2126=CYLINDRICAL_SURFACE('',#2616,7.);
#2127=CYLINDRICAL_SURFACE('',#2620,7.);
#2128=CYLINDRICAL_SURFACE('',#2623,7.);
#2129=CYLINDRICAL_SURFACE('',#2626,7.);
#2130=CYLINDRICAL_SURFACE('',#2630,15.);
#2131=CYLINDRICAL_SURFACE('',#2634,15.);
#2132=CYLINDRICAL_SURFACE('',#2640,7.);
#2133=CYLINDRICAL_SURFACE('',#2643,7.);
#2134=CYLINDRICAL_SURFACE('',#2647,12.);
#2135=CYLINDRICAL_SURFACE('',#2651,12.);
#2136=CYLINDRICAL_SURFACE('',#2657,5.);
#2137=CYLINDRICAL_SURFACE('',#2667,5.);
#2138=CYLINDRICAL_SURFACE('',#2670,5.);
#2139=CYLINDRICAL_SURFACE('',#2673,5.);
#2140=CYLINDRICAL_SURFACE('',#2683,5.);
#2141=CYLINDRICAL_SURFACE('',#2686,12.);
#2142=CYLINDRICAL_SURFACE('',#2692,5.);
#2143=CYLINDRICAL_SURFACE('',#2702,4.);
#2144=CYLINDRICAL_SURFACE('',#2709,5.);
#2145=CYLINDRICAL_SURFACE('',#2714,8.);
#2146=CYLINDRICAL_SURFACE('',#2717,5.);
#2147=CYLINDRICAL_SURFACE('',#2720,4.);
#2148=CYLINDRICAL_SURFACE('',#2727,5.);
#2149=CYLINDRICAL_SURFACE('',#2732,8.);
#2150=CYLINDRICAL_SURFACE('',#2735,5.);
#2151=CYLINDRICAL_SURFACE('',#2738,4.);
#2152=CYLINDRICAL_SURFACE('',#2745,5.);
#2153=CYLINDRICAL_SURFACE('',#2750,8.);
#2154=CYLINDRICAL_SURFACE('',#2753,5.);
#2155=CYLINDRICAL_SURFACE('',#2762,7.);
#2156=CYLINDRICAL_SURFACE('',#2763,5.);
#2157=CYLINDRICAL_SURFACE('',#2765,4.);
#2158=CYLINDRICAL_SURFACE('',#2772,5.);
#2159=CYLINDRICAL_SURFACE('',#2776,8.);
#2160=CYLINDRICAL_SURFACE('',#2779,5.);
#2161=CYLINDRICAL_SURFACE('',#2782,4.);
#2162=CYLINDRICAL_SURFACE('',#2789,5.);
#2163=CYLINDRICAL_SURFACE('',#2794,8.);
#2164=CYLINDRICAL_SURFACE('',#2797,5.);
#2165=CYLINDRICAL_SURFACE('',#2800,4.);
#2166=CYLINDRICAL_SURFACE('',#2807,5.);
#2167=CYLINDRICAL_SURFACE('',#2812,8.);
#2168=CYLINDRICAL_SURFACE('',#2815,5.);
#2169=CYLINDRICAL_SURFACE('',#2818,5.);
#2170=CYLINDRICAL_SURFACE('',#2821,7.);
#2171=CYLINDRICAL_SURFACE('',#2827,5.);
#2172=CYLINDRICAL_SURFACE('',#2830,7.);
#2173=CYLINDRICAL_SURFACE('',#2836,5.);
#2174=CYLINDRICAL_SURFACE('',#2839,10.);
#2175=CYLINDRICAL_SURFACE('',#2850,4.);
#2176=CYLINDRICAL_SURFACE('',#2852,8.);
#2177=ADVANCED_FACE('',(#405),#2116,.F.);
#2178=ADVANCED_FACE('',(#406),#2117,.F.);
#2179=ADVANCED_FACE('',(#407),#319,.T.);
#2180=ADVANCED_FACE('',(#408),#320,.T.);
#2181=ADVANCED_FACE('',(#409),#321,.T.);
#2182=ADVANCED_FACE('',(#410),#322,.T.);
#2183=ADVANCED_FACE('',(#411,#259,#260),#323,.T.);
#2184=ADVANCED_FACE('',(#412,#261,#262),#324,.F.);
#2185=ADVANCED_FACE('',(#413),#2118,.F.);
#2186=ADVANCED_FACE('',(#414),#2119,.T.);
#2187=ADVANCED_FACE('',(#415,#263),#325,.T.);
#2188=ADVANCED_FACE('',(#416,#264),#326,.F.);
#2189=ADVANCED_FACE('',(#417),#2120,.F.);
#2190=ADVANCED_FACE('',(#418),#2121,.T.);
#2191=ADVANCED_FACE('',(#419,#265),#327,.T.);
#2192=ADVANCED_FACE('',(#420,#266),#328,.F.);
#2193=ADVANCED_FACE('',(#421),#2122,.F.);
#2194=ADVANCED_FACE('',(#422),#2123,.F.);
#2195=ADVANCED_FACE('',(#423),#329,.T.);
#2196=ADVANCED_FACE('',(#424),#2124,.T.);
#2197=ADVANCED_FACE('',(#425),#330,.T.);
#2198=ADVANCED_FACE('',(#426),#2125,.T.);
#2199=ADVANCED_FACE('',(#427,#267,#268),#331,.T.);
#2200=ADVANCED_FACE('',(#428,#269,#270),#332,.F.);
#2201=ADVANCED_FACE('',(#429),#333,.F.);
#2202=ADVANCED_FACE('',(#430),#2126,.F.);
#2203=ADVANCED_FACE('',(#431),#334,.F.);
#2204=ADVANCED_FACE('',(#432),#2127,.F.);
#2205=ADVANCED_FACE('',(#433),#2128,.F.);
#2206=ADVANCED_FACE('',(#434),#2129,.F.);
#2207=ADVANCED_FACE('',(#435),#335,.T.);
#2208=ADVANCED_FACE('',(#436),#2130,.T.);
#2209=ADVANCED_FACE('',(#437),#336,.T.);
#2210=ADVANCED_FACE('',(#438),#2131,.T.);
#2211=ADVANCED_FACE('',(#439,#271,#272,#273),#337,.T.);
#2212=ADVANCED_FACE('',(#440,#274,#275,#276),#338,.F.);
#2213=ADVANCED_FACE('',(#441),#2132,.F.);
#2214=ADVANCED_FACE('',(#442),#2133,.F.);
#2215=ADVANCED_FACE('',(#443),#339,.T.);
#2216=ADVANCED_FACE('',(#444),#2134,.T.);
#2217=ADVANCED_FACE('',(#445),#340,.T.);
#2218=ADVANCED_FACE('',(#446),#2135,.T.);
#2219=ADVANCED_FACE('',(#447,#277,#278),#341,.T.);
#2220=ADVANCED_FACE('',(#448,#279,#280),#342,.F.);
#2221=ADVANCED_FACE('',(#449),#2136,.F.);
#2222=ADVANCED_FACE('',(#450),#343,.T.);
#2223=ADVANCED_FACE('',(#451),#344,.T.);
#2224=ADVANCED_FACE('',(#452),#345,.T.);
#2225=ADVANCED_FACE('',(#453),#346,.T.);
#2226=ADVANCED_FACE('',(#454,#281),#347,.T.);
#2227=ADVANCED_FACE('',(#455,#282),#348,.F.);
#2228=ADVANCED_FACE('',(#456),#2137,.F.);
#2229=ADVANCED_FACE('',(#457),#2138,.F.);
#2230=ADVANCED_FACE('',(#458),#2139,.F.);
#2231=ADVANCED_FACE('',(#459,#283,#284),#349,.T.);
#2232=ADVANCED_FACE('',(#460),#350,.T.);
#2233=ADVANCED_FACE('',(#461,#285,#286),#351,.T.);
#2234=ADVANCED_FACE('',(#462),#352,.T.);
#2235=ADVANCED_FACE('',(#463,#287),#353,.T.);
#2236=ADVANCED_FACE('',(#464,#288),#354,.F.);
#2237=ADVANCED_FACE('',(#465),#2140,.F.);
#2238=ADVANCED_FACE('',(#466),#2141,.T.);
#2239=ADVANCED_FACE('',(#467,#289),#355,.T.);
#2240=ADVANCED_FACE('',(#468,#290),#356,.F.);
#2241=ADVANCED_FACE('',(#469),#2142,.F.);
#2242=ADVANCED_FACE('',(#470,#291),#357,.T.);
#2243=ADVANCED_FACE('',(#471),#358,.T.);
#2244=ADVANCED_FACE('',(#472,#292),#359,.T.);
#2245=ADVANCED_FACE('',(#473),#360,.T.);
#2246=ADVANCED_FACE('',(#474),#361,.T.);
#2247=ADVANCED_FACE('',(#475),#362,.F.);
#2248=ADVANCED_FACE('',(#476),#2143,.T.);
#2249=ADVANCED_FACE('',(#477,#293),#363,.F.);
#2250=ADVANCED_FACE('',(#478,#294),#364,.F.);
#2251=ADVANCED_FACE('',(#479),#2144,.T.);
#2252=ADVANCED_FACE('',(#480,#295),#365,.T.);
#2253=ADVANCED_FACE('',(#481),#2145,.T.);
#2254=ADVANCED_FACE('',(#482),#366,.F.);
#2255=ADVANCED_FACE('',(#483),#2146,.T.);
#2256=ADVANCED_FACE('',(#484),#367,.T.);
#2257=ADVANCED_FACE('',(#485),#2147,.T.);
#2258=ADVANCED_FACE('',(#486,#296),#368,.F.);
#2259=ADVANCED_FACE('',(#487,#297),#369,.F.);
#2260=ADVANCED_FACE('',(#488),#2148,.T.);
#2261=ADVANCED_FACE('',(#489,#298),#370,.T.);
#2262=ADVANCED_FACE('',(#490),#2149,.T.);
#2263=ADVANCED_FACE('',(#491),#371,.F.);
#2264=ADVANCED_FACE('',(#492),#2150,.T.);
#2265=ADVANCED_FACE('',(#493),#372,.T.);
#2266=ADVANCED_FACE('',(#494),#2151,.T.);
#2267=ADVANCED_FACE('',(#495,#299),#373,.F.);
#2268=ADVANCED_FACE('',(#496,#300),#374,.F.);
#2269=ADVANCED_FACE('',(#497),#2152,.T.);
#2270=ADVANCED_FACE('',(#498,#301),#375,.T.);
#2271=ADVANCED_FACE('',(#499),#2153,.T.);
#2272=ADVANCED_FACE('',(#500),#376,.F.);
#2273=ADVANCED_FACE('',(#501),#2154,.T.);
#2274=ADVANCED_FACE('',(#502),#377,.T.);
#2275=ADVANCED_FACE('',(#503,#302),#378,.T.);
#2276=ADVANCED_FACE('',(#504,#303),#379,.F.);
#2277=ADVANCED_FACE('',(#505),#2155,.T.);
#2278=ADVANCED_FACE('',(#506),#2156,.T.);
#2279=ADVANCED_FACE('',(#507),#2157,.T.);
#2280=ADVANCED_FACE('',(#508,#304),#380,.F.);
#2281=ADVANCED_FACE('',(#509,#305),#381,.F.);
#2282=ADVANCED_FACE('',(#510),#2158,.T.);
#2283=ADVANCED_FACE('',(#511,#306),#382,.T.);
#2284=ADVANCED_FACE('',(#512),#2159,.T.);
#2285=ADVANCED_FACE('',(#513),#383,.F.);
#2286=ADVANCED_FACE('',(#514),#2160,.T.);
#2287=ADVANCED_FACE('',(#515),#384,.T.);
#2288=ADVANCED_FACE('',(#516),#2161,.T.);
#2289=ADVANCED_FACE('',(#517,#307),#385,.F.);
#2290=ADVANCED_FACE('',(#518,#308),#386,.F.);
#2291=ADVANCED_FACE('',(#519),#2162,.T.);
#2292=ADVANCED_FACE('',(#520,#309),#387,.T.);
#2293=ADVANCED_FACE('',(#521),#2163,.T.);
#2294=ADVANCED_FACE('',(#522),#388,.F.);
#2295=ADVANCED_FACE('',(#523),#2164,.T.);
#2296=ADVANCED_FACE('',(#524),#389,.T.);
#2297=ADVANCED_FACE('',(#525),#2165,.T.);
#2298=ADVANCED_FACE('',(#526,#310),#390,.F.);
#2299=ADVANCED_FACE('',(#527,#311),#391,.F.);
#2300=ADVANCED_FACE('',(#528),#2166,.T.);
#2301=ADVANCED_FACE('',(#529,#312),#392,.T.);
#2302=ADVANCED_FACE('',(#530),#2167,.T.);
#2303=ADVANCED_FACE('',(#531),#393,.F.);
#2304=ADVANCED_FACE('',(#532),#2168,.T.);
#2305=ADVANCED_FACE('',(#533),#394,.T.);
#2306=ADVANCED_FACE('',(#534),#2169,.F.);
#2307=ADVANCED_FACE('',(#535),#2170,.T.);
#2308=ADVANCED_FACE('',(#536,#313),#395,.T.);
#2309=ADVANCED_FACE('',(#537,#314),#396,.F.);
#2310=ADVANCED_FACE('',(#538),#2171,.F.);
#2311=ADVANCED_FACE('',(#539),#2172,.T.);
#2312=ADVANCED_FACE('',(#540,#315),#397,.T.);
#2313=ADVANCED_FACE('',(#541,#316),#398,.F.);
#2314=ADVANCED_FACE('',(#542),#2173,.F.);
#2315=ADVANCED_FACE('',(#543),#2174,.T.);
#2316=ADVANCED_FACE('',(#544,#317),#399,.T.);
#2317=ADVANCED_FACE('',(#545,#318),#400,.F.);
#2318=ADVANCED_FACE('',(#546),#401,.F.);
#2319=ADVANCED_FACE('',(#547),#402,.F.);
#2320=ADVANCED_FACE('',(#548),#403,.F.);
#2321=ADVANCED_FACE('',(#549),#2175,.F.);
#2322=ADVANCED_FACE('',(#550),#2176,.T.);
#2323=ADVANCED_FACE('',(#551),#404,.T.);
#2324=CLOSED_SHELL('',(#2177,#2178,#2179,#2180,#2181,#2182,#2183,#2184));
#2325=CLOSED_SHELL('',(#2185,#2186,#2187,#2188));
#2326=CLOSED_SHELL('',(#2189,#2190,#2191,#2192));
#2327=CLOSED_SHELL('',(#2193,#2194,#2195,#2196,#2197,#2198,#2199,#2200));
#2328=CLOSED_SHELL('',(#2201,#2202,#2203,#2204,#2205,#2206,#2207,#2208,
#2209,#2210,#2211,#2212));
#2329=CLOSED_SHELL('',(#2213,#2214,#2215,#2216,#2217,#2218,#2219,#2220));
#2330=CLOSED_SHELL('',(#2221,#2222,#2223,#2224,#2225,#2226,#2227));
#2331=CLOSED_SHELL('',(#2228,#2229,#2230,#2231,#2232,#2233,#2234,#2235,
#2236));
#2332=CLOSED_SHELL('',(#2237,#2238,#2239,#2240));
#2333=CLOSED_SHELL('',(#2241,#2242,#2243,#2244,#2245,#2246,#2247));
#2334=CLOSED_SHELL('',(#2248,#2249,#2250,#2251,#2252,#2253,#2254,#2255,
#2256));
#2335=CLOSED_SHELL('',(#2257,#2258,#2259,#2260,#2261,#2262,#2263,#2264,
#2265));
#2336=CLOSED_SHELL('',(#2266,#2267,#2268,#2269,#2270,#2271,#2272,#2273,
#2274));
#2337=CLOSED_SHELL('',(#2275,#2276,#2277,#2278,#2279,#2280,#2281,#2282,
#2283,#2284,#2285,#2286,#2287));
#2338=CLOSED_SHELL('',(#2288,#2289,#2290,#2291,#2292,#2293,#2294,#2295,
#2296));
#2339=CLOSED_SHELL('',(#2297,#2298,#2299,#2300,#2301,#2302,#2303,#2304,
#2305));
#2340=CLOSED_SHELL('',(#2306,#2307,#2308,#2309));
#2341=CLOSED_SHELL('',(#2310,#2311,#2312,#2313));
#2342=CLOSED_SHELL('',(#2314,#2315,#2316,#2317));
#2343=CLOSED_SHELL('',(#2318,#2319,#2320,#2321,#2322,#2323));
#2344=DERIVED_UNIT_ELEMENT(#2384,1.);
#2345=DERIVED_UNIT_ELEMENT(#4390,-3.);
#2346=DERIVED_UNIT_ELEMENT(#2384,1.);
#2347=DERIVED_UNIT_ELEMENT(#4390,-3.);
#2348=DERIVED_UNIT_ELEMENT(#2384,1.);
#2349=DERIVED_UNIT_ELEMENT(#4390,-3.);
#2350=DERIVED_UNIT_ELEMENT(#2384,1.);
#2351=DERIVED_UNIT_ELEMENT(#4390,-3.);
#2352=DERIVED_UNIT_ELEMENT(#2384,1.);
#2353=DERIVED_UNIT_ELEMENT(#4390,-3.);
#2354=DERIVED_UNIT_ELEMENT(#2384,1.);
#2355=DERIVED_UNIT_ELEMENT(#4390,-3.);
#2356=DERIVED_UNIT_ELEMENT(#2384,1.);
#2357=DERIVED_UNIT_ELEMENT(#4390,-3.);
#2358=DERIVED_UNIT_ELEMENT(#2384,1.);
#2359=DERIVED_UNIT_ELEMENT(#4390,-3.);
#2360=DERIVED_UNIT_ELEMENT(#2384,1.);
#2361=DERIVED_UNIT_ELEMENT(#4390,-3.);
#2362=DERIVED_UNIT_ELEMENT(#2384,1.);
#2363=DERIVED_UNIT_ELEMENT(#4390,-3.);
#2364=DERIVED_UNIT_ELEMENT(#2384,1.);
#2365=DERIVED_UNIT_ELEMENT(#4390,-3.);
#2366=DERIVED_UNIT_ELEMENT(#2384,1.);
#2367=DERIVED_UNIT_ELEMENT(#4390,-3.);
#2368=DERIVED_UNIT_ELEMENT(#2384,1.);
#2369=DERIVED_UNIT_ELEMENT(#4390,-3.);
#2370=DERIVED_UNIT_ELEMENT(#2384,1.);
#2371=DERIVED_UNIT_ELEMENT(#4390,-3.);
#2372=DERIVED_UNIT_ELEMENT(#2384,1.);
#2373=DERIVED_UNIT_ELEMENT(#4390,-3.);
#2374=DERIVED_UNIT_ELEMENT(#2384,1.);
#2375=DERIVED_UNIT_ELEMENT(#4390,-3.);
#2376=DERIVED_UNIT_ELEMENT(#2384,1.);
#2377=DERIVED_UNIT_ELEMENT(#4390,-3.);
#2378=DERIVED_UNIT_ELEMENT(#2384,1.);
#2379=DERIVED_UNIT_ELEMENT(#4390,-3.);
#2380=DERIVED_UNIT_ELEMENT(#2384,1.);
#2381=DERIVED_UNIT_ELEMENT(#4390,-3.);
#2382=DERIVED_UNIT_ELEMENT(#2384,1.);
#2383=DERIVED_UNIT_ELEMENT(#4390,-3.);
#2384=(
MASS_UNIT()
NAMED_UNIT(*)
SI_UNIT(.KILO.,.GRAM.)
);
#2385=DERIVED_UNIT((#2344,#2345));
#2386=DERIVED_UNIT((#2346,#2347));
#2387=DERIVED_UNIT((#2348,#2349));
#2388=DERIVED_UNIT((#2350,#2351));
#2389=DERIVED_UNIT((#2352,#2353));
#2390=DERIVED_UNIT((#2354,#2355));
#2391=DERIVED_UNIT((#2356,#2357));
#2392=DERIVED_UNIT((#2358,#2359));
#2393=DERIVED_UNIT((#2360,#2361));
#2394=DERIVED_UNIT((#2362,#2363));
#2395=DERIVED_UNIT((#2364,#2365));
#2396=DERIVED_UNIT((#2366,#2367));
#2397=DERIVED_UNIT((#2368,#2369));
#2398=DERIVED_UNIT((#2370,#2371));
#2399=DERIVED_UNIT((#2372,#2373));
#2400=DERIVED_UNIT((#2374,#2375));
#2401=DERIVED_UNIT((#2376,#2377));
#2402=DERIVED_UNIT((#2378,#2379));
#2403=DERIVED_UNIT((#2380,#2381));
#2404=DERIVED_UNIT((#2382,#2383));
#2405=MEASURE_REPRESENTATION_ITEM('density measure',
POSITIVE_RATIO_MEASURE(7850.),#2385);
#2406=MEASURE_REPRESENTATION_ITEM('density measure',
POSITIVE_RATIO_MEASURE(7850.),#2386);
#2407=MEASURE_REPRESENTATION_ITEM('density measure',
POSITIVE_RATIO_MEASURE(7850.),#2387);
#2408=MEASURE_REPRESENTATION_ITEM('density measure',
POSITIVE_RATIO_MEASURE(7850.),#2388);
#2409=MEASURE_REPRESENTATION_ITEM('density measure',
POSITIVE_RATIO_MEASURE(7850.),#2389);
#2410=MEASURE_REPRESENTATION_ITEM('density measure',
POSITIVE_RATIO_MEASURE(7850.),#2390);
#2411=MEASURE_REPRESENTATION_ITEM('density measure',
POSITIVE_RATIO_MEASURE(8920.),#2391);
#2412=MEASURE_REPRESENTATION_ITEM('density measure',
POSITIVE_RATIO_MEASURE(7850.),#2392);
#2413=MEASURE_REPRESENTATION_ITEM('density measure',
POSITIVE_RATIO_MEASURE(7850.),#2393);
#2414=MEASURE_REPRESENTATION_ITEM('density measure',
POSITIVE_RATIO_MEASURE(7850.),#2394);
#2415=MEASURE_REPRESENTATION_ITEM('density measure',
POSITIVE_RATIO_MEASURE(7850.),#2395);
#2416=MEASURE_REPRESENTATION_ITEM('density measure',
POSITIVE_RATIO_MEASURE(7850.),#2396);
#2417=MEASURE_REPRESENTATION_ITEM('density measure',
POSITIVE_RATIO_MEASURE(7850.),#2397);
#2418=MEASURE_REPRESENTATION_ITEM('density measure',
POSITIVE_RATIO_MEASURE(7850.),#2398);
#2419=MEASURE_REPRESENTATION_ITEM('density measure',
POSITIVE_RATIO_MEASURE(7850.),#2399);
#2420=MEASURE_REPRESENTATION_ITEM('density measure',
POSITIVE_RATIO_MEASURE(7850.),#2400);
#2421=MEASURE_REPRESENTATION_ITEM('density measure',
POSITIVE_RATIO_MEASURE(8920.),#2401);
#2422=MEASURE_REPRESENTATION_ITEM('density measure',
POSITIVE_RATIO_MEASURE(8920.),#2402);
#2423=MEASURE_REPRESENTATION_ITEM('density measure',
POSITIVE_RATIO_MEASURE(7850.),#2403);
#2424=MEASURE_REPRESENTATION_ITEM('density measure',
POSITIVE_RATIO_MEASURE(7850.),#2404);
#2425=PROPERTY_DEFINITION_REPRESENTATION(#2525,#2465);
#2426=PROPERTY_DEFINITION_REPRESENTATION(#2526,#2466);
#2427=PROPERTY_DEFINITION_REPRESENTATION(#2527,#2467);
#2428=PROPERTY_DEFINITION_REPRESENTATION(#2528,#2468);
#2429=PROPERTY_DEFINITION_REPRESENTATION(#2529,#2469);
#2430=PROPERTY_DEFINITION_REPRESENTATION(#2530,#2470);
#2431=PROPERTY_DEFINITION_REPRESENTATION(#2531,#2471);
#2432=PROPERTY_DEFINITION_REPRESENTATION(#2532,#2472);
#2433=PROPERTY_DEFINITION_REPRESENTATION(#2533,#2473);
#2434=PROPERTY_DEFINITION_REPRESENTATION(#2534,#2474);
#2435=PROPERTY_DEFINITION_REPRESENTATION(#2535,#2475);
#2436=PROPERTY_DEFINITION_REPRESENTATION(#2536,#2476);
#2437=PROPERTY_DEFINITION_REPRESENTATION(#2537,#2477);
#2438=PROPERTY_DEFINITION_REPRESENTATION(#2538,#2478);
#2439=PROPERTY_DEFINITION_REPRESENTATION(#2539,#2479);
#2440=PROPERTY_DEFINITION_REPRESENTATION(#2540,#2480);
#2441=PROPERTY_DEFINITION_REPRESENTATION(#2541,#2481);
#2442=PROPERTY_DEFINITION_REPRESENTATION(#2542,#2482);
#2443=PROPERTY_DEFINITION_REPRESENTATION(#2543,#2483);
#2444=PROPERTY_DEFINITION_REPRESENTATION(#2544,#2484);
#2445=PROPERTY_DEFINITION_REPRESENTATION(#2545,#2485);
#2446=PROPERTY_DEFINITION_REPRESENTATION(#2546,#2486);
#2447=PROPERTY_DEFINITION_REPRESENTATION(#2547,#2487);
#2448=PROPERTY_DEFINITION_REPRESENTATION(#2548,#2488);
#2449=PROPERTY_DEFINITION_REPRESENTATION(#2549,#2489);
#2450=PROPERTY_DEFINITION_REPRESENTATION(#2550,#2490);
#2451=PROPERTY_DEFINITION_REPRESENTATION(#2551,#2491);
#2452=PROPERTY_DEFINITION_REPRESENTATION(#2552,#2492);
#2453=PROPERTY_DEFINITION_REPRESENTATION(#2553,#2493);
#2454=PROPERTY_DEFINITION_REPRESENTATION(#2554,#2494);
#2455=PROPERTY_DEFINITION_REPRESENTATION(#2555,#2495);
#2456=PROPERTY_DEFINITION_REPRESENTATION(#2556,#2496);
#2457=PROPERTY_DEFINITION_REPRESENTATION(#2557,#2497);
#2458=PROPERTY_DEFINITION_REPRESENTATION(#2558,#2498);
#2459=PROPERTY_DEFINITION_REPRESENTATION(#2559,#2499);
#2460=PROPERTY_DEFINITION_REPRESENTATION(#2560,#2500);
#2461=PROPERTY_DEFINITION_REPRESENTATION(#2561,#2501);
#2462=PROPERTY_DEFINITION_REPRESENTATION(#2562,#2502);
#2463=PROPERTY_DEFINITION_REPRESENTATION(#2563,#2503);
#2464=PROPERTY_DEFINITION_REPRESENTATION(#2564,#2504);
#2465=REPRESENTATION('material name',(#2505),#4368);
#2466=REPRESENTATION('density',(#2405),#4368);
#2467=REPRESENTATION('material name',(#2506),#4369);
#2468=REPRESENTATION('density',(#2406),#4369);
#2469=REPRESENTATION('material name',(#2507),#4370);
#2470=REPRESENTATION('density',(#2407),#4370);
#2471=REPRESENTATION('material name',(#2508),#4371);
#2472=REPRESENTATION('density',(#2408),#4371);
#2473=REPRESENTATION('material name',(#2509),#4372);
#2474=REPRESENTATION('density',(#2409),#4372);
#2475=REPRESENTATION('material name',(#2510),#4373);
#2476=REPRESENTATION('density',(#2410),#4373);
#2477=REPRESENTATION('material name',(#2511),#4374);
#2478=REPRESENTATION('density',(#2411),#4374);
#2479=REPRESENTATION('material name',(#2512),#4375);
#2480=REPRESENTATION('density',(#2412),#4375);
#2481=REPRESENTATION('material name',(#2513),#4376);
#2482=REPRESENTATION('density',(#2413),#4376);
#2483=REPRESENTATION('material name',(#2514),#4377);
#2484=REPRESENTATION('density',(#2414),#4377);
#2485=REPRESENTATION('material name',(#2515),#4378);
#2486=REPRESENTATION('density',(#2415),#4378);
#2487=REPRESENTATION('material name',(#2516),#4379);
#2488=REPRESENTATION('density',(#2416),#4379);
#2489=REPRESENTATION('material name',(#2517),#4380);
#2490=REPRESENTATION('density',(#2417),#4380);
#2491=REPRESENTATION('material name',(#2518),#4381);
#2492=REPRESENTATION('density',(#2418),#4381);
#2493=REPRESENTATION('material name',(#2519),#4382);
#2494=REPRESENTATION('density',(#2419),#4382);
#2495=REPRESENTATION('material name',(#2520),#4383);
#2496=REPRESENTATION('density',(#2420),#4383);
#2497=REPRESENTATION('material name',(#2521),#4384);
#2498=REPRESENTATION('density',(#2421),#4384);
#2499=REPRESENTATION('material name',(#2522),#4385);
#2500=REPRESENTATION('density',(#2422),#4385);
#2501=REPRESENTATION('material name',(#2523),#4386);
#2502=REPRESENTATION('density',(#2423),#4386);
#2503=REPRESENTATION('material name',(#2524),#4387);
#2504=REPRESENTATION('density',(#2424),#4387);
#2505=DESCRIPTIVE_REPRESENTATION_ITEM('Steel','Steel');
#2506=DESCRIPTIVE_REPRESENTATION_ITEM('Steel','Steel');
#2507=DESCRIPTIVE_REPRESENTATION_ITEM('Steel','Steel');
#2508=DESCRIPTIVE_REPRESENTATION_ITEM('Steel','Steel');
#2509=DESCRIPTIVE_REPRESENTATION_ITEM('Steel','Steel');
#2510=DESCRIPTIVE_REPRESENTATION_ITEM('Steel','Steel');
#2511=DESCRIPTIVE_REPRESENTATION_ITEM('Copper, Alloy','Copper, Alloy');
#2512=DESCRIPTIVE_REPRESENTATION_ITEM('Steel','Steel');
#2513=DESCRIPTIVE_REPRESENTATION_ITEM('Steel','Steel');
#2514=DESCRIPTIVE_REPRESENTATION_ITEM('Steel','Steel');
#2515=DESCRIPTIVE_REPRESENTATION_ITEM('Steel','Steel');
#2516=DESCRIPTIVE_REPRESENTATION_ITEM('Steel','Steel');
#2517=DESCRIPTIVE_REPRESENTATION_ITEM('Steel','Steel');
#2518=DESCRIPTIVE_REPRESENTATION_ITEM('Steel','Steel');
#2519=DESCRIPTIVE_REPRESENTATION_ITEM('Steel','Steel');
#2520=DESCRIPTIVE_REPRESENTATION_ITEM('Steel','Steel');
#2521=DESCRIPTIVE_REPRESENTATION_ITEM('Copper, Alloy','Copper, Alloy');
#2522=DESCRIPTIVE_REPRESENTATION_ITEM('Copper, Alloy','Copper, Alloy');
#2523=DESCRIPTIVE_REPRESENTATION_ITEM('Steel','Steel');
#2524=DESCRIPTIVE_REPRESENTATION_ITEM('Steel','Steel');
#2525=PROPERTY_DEFINITION('material property','material name',#4500);
#2526=PROPERTY_DEFINITION('material property','density of part',#4500);
#2527=PROPERTY_DEFINITION('material property','material name',#4501);
#2528=PROPERTY_DEFINITION('material property','density of part',#4501);
#2529=PROPERTY_DEFINITION('material property','material name',#4502);
#2530=PROPERTY_DEFINITION('material property','density of part',#4502);
#2531=PROPERTY_DEFINITION('material property','material name',#4503);
#2532=PROPERTY_DEFINITION('material property','density of part',#4503);
#2533=PROPERTY_DEFINITION('material property','material name',#4504);
#2534=PROPERTY_DEFINITION('material property','density of part',#4504);
#2535=PROPERTY_DEFINITION('material property','material name',#4505);
#2536=PROPERTY_DEFINITION('material property','density of part',#4505);
#2537=PROPERTY_DEFINITION('material property','material name',#4506);
#2538=PROPERTY_DEFINITION('material property','density of part',#4506);
#2539=PROPERTY_DEFINITION('material property','material name',#4507);
#2540=PROPERTY_DEFINITION('material property','density of part',#4507);
#2541=PROPERTY_DEFINITION('material property','material name',#4508);
#2542=PROPERTY_DEFINITION('material property','density of part',#4508);
#2543=PROPERTY_DEFINITION('material property','material name',#4509);
#2544=PROPERTY_DEFINITION('material property','density of part',#4509);
#2545=PROPERTY_DEFINITION('material property','material name',#4510);
#2546=PROPERTY_DEFINITION('material property','density of part',#4510);
#2547=PROPERTY_DEFINITION('material property','material name',#4511);
#2548=PROPERTY_DEFINITION('material property','density of part',#4511);
#2549=PROPERTY_DEFINITION('material property','material name',#4512);
#2550=PROPERTY_DEFINITION('material property','density of part',#4512);
#2551=PROPERTY_DEFINITION('material property','material name',#4513);
#2552=PROPERTY_DEFINITION('material property','density of part',#4513);
#2553=PROPERTY_DEFINITION('material property','material name',#4514);
#2554=PROPERTY_DEFINITION('material property','density of part',#4514);
#2555=PROPERTY_DEFINITION('material property','material name',#4515);
#2556=PROPERTY_DEFINITION('material property','density of part',#4515);
#2557=PROPERTY_DEFINITION('material property','material name',#4516);
#2558=PROPERTY_DEFINITION('material property','density of part',#4516);
#2559=PROPERTY_DEFINITION('material property','material name',#4517);
#2560=PROPERTY_DEFINITION('material property','density of part',#4517);
#2561=PROPERTY_DEFINITION('material property','material name',#4518);
#2562=PROPERTY_DEFINITION('material property','density of part',#4518);
#2563=PROPERTY_DEFINITION('material property','material name',#4519);
#2564=PROPERTY_DEFINITION('material property','density of part',#4519);
#2565=AXIS2_PLACEMENT_3D('',#3700,#2897,#2898);
#2566=AXIS2_PLACEMENT_3D('',#3701,#2899,#2900);
#2567=AXIS2_PLACEMENT_3D('',#3702,#2901,#2902);
#2568=AXIS2_PLACEMENT_3D('',#3704,#2903,#2904);
#2569=AXIS2_PLACEMENT_3D('',#3707,#2906,#2907);
#2570=AXIS2_PLACEMENT_3D('',#3708,#2908,#2909);
#2571=AXIS2_PLACEMENT_3D('',#3710,#2910,#2911);
#2572=AXIS2_PLACEMENT_3D('',#3713,#2913,#2914);
#2573=AXIS2_PLACEMENT_3D('',#3714,#2915,#2916);
#2574=AXIS2_PLACEMENT_3D('',#3723,#2921,#2922);
#2575=AXIS2_PLACEMENT_3D('',#3729,#2926,#2927);
#2576=AXIS2_PLACEMENT_3D('',#3735,#2931,#2932);
#2577=AXIS2_PLACEMENT_3D('',#3738,#2935,#2936);
#2578=AXIS2_PLACEMENT_3D('',#3739,#2937,#2938);
#2579=AXIS2_PLACEMENT_3D('',#3740,#2939,#2940);
#2580=AXIS2_PLACEMENT_3D('',#3741,#2941,#2942);
#2581=AXIS2_PLACEMENT_3D('',#3743,#2943,#2944);
#2582=AXIS2_PLACEMENT_3D('',#3746,#2946,#2947);
#2583=AXIS2_PLACEMENT_3D('',#3747,#2948,#2949);
#2584=AXIS2_PLACEMENT_3D('',#3749,#2950,#2951);
#2585=AXIS2_PLACEMENT_3D('',#3752,#2953,#2954);
#2586=AXIS2_PLACEMENT_3D('',#3753,#2955,#2956);
#2587=AXIS2_PLACEMENT_3D('',#3754,#2957,#2958);
#2588=AXIS2_PLACEMENT_3D('',#3755,#2959,#2960);
#2589=AXIS2_PLACEMENT_3D('',#3756,#2961,#2962);
#2590=AXIS2_PLACEMENT_3D('',#3758,#2963,#2964);
#2591=AXIS2_PLACEMENT_3D('',#3761,#2966,#2967);
#2592=AXIS2_PLACEMENT_3D('',#3762,#2968,#2969);
#2593=AXIS2_PLACEMENT_3D('',#3764,#2970,#2971);
#2594=AXIS2_PLACEMENT_3D('',#3767,#2973,#2974);
#2595=AXIS2_PLACEMENT_3D('',#3768,#2975,#2976);
#2596=AXIS2_PLACEMENT_3D('',#3769,#2977,#2978);
#2597=AXIS2_PLACEMENT_3D('',#3770,#2979,#2980);
#2598=AXIS2_PLACEMENT_3D('',#3771,#2981,#2982);
#2599=AXIS2_PLACEMENT_3D('',#3773,#2983,#2984);
#2600=AXIS2_PLACEMENT_3D('',#3776,#2986,#2987);
#2601=AXIS2_PLACEMENT_3D('',#3777,#2988,#2989);
#2602=AXIS2_PLACEMENT_3D('',#3779,#2990,#2991);
#2603=AXIS2_PLACEMENT_3D('',#3782,#2993,#2994);
#2604=AXIS2_PLACEMENT_3D('',#3783,#2995,#2996);
#2605=AXIS2_PLACEMENT_3D('',#3792,#3001,#3002);
#2606=AXIS2_PLACEMENT_3D('',#3794,#3003,#3004);
#2607=AXIS2_PLACEMENT_3D('',#3796,#3005,#3006);
#2608=AXIS2_PLACEMENT_3D('',#3798,#3008,#3009);
#2609=AXIS2_PLACEMENT_3D('',#3804,#3013,#3014);
#2610=AXIS2_PLACEMENT_3D('',#3805,#3015,#3016);
#2611=AXIS2_PLACEMENT_3D('',#3806,#3017,#3018);
#2612=AXIS2_PLACEMENT_3D('',#3807,#3019,#3020);
#2613=AXIS2_PLACEMENT_3D('',#3808,#3021,#3022);
#2614=AXIS2_PLACEMENT_3D('',#3809,#3023,#3024);
#2615=AXIS2_PLACEMENT_3D('',#3810,#3025,#3026);
#2616=AXIS2_PLACEMENT_3D('',#3819,#3031,#3032);
#2617=AXIS2_PLACEMENT_3D('',#3821,#3033,#3034);
#2618=AXIS2_PLACEMENT_3D('',#3824,#3036,#3037);
#2619=AXIS2_PLACEMENT_3D('',#3825,#3038,#3039);
#2620=AXIS2_PLACEMENT_3D('',#3831,#3043,#3044);
#2621=AXIS2_PLACEMENT_3D('',#3832,#3045,#3046);
#2622=AXIS2_PLACEMENT_3D('',#3833,#3047,#3048);
#2623=AXIS2_PLACEMENT_3D('',#3834,#3049,#3050);
#2624=AXIS2_PLACEMENT_3D('',#3836,#3051,#3052);
#2625=AXIS2_PLACEMENT_3D('',#3839,#3054,#3055);
#2626=AXIS2_PLACEMENT_3D('',#3840,#3056,#3057);
#2627=AXIS2_PLACEMENT_3D('',#3842,#3058,#3059);
#2628=AXIS2_PLACEMENT_3D('',#3845,#3061,#3062);
#2629=AXIS2_PLACEMENT_3D('',#3846,#3063,#3064);
#2630=AXIS2_PLACEMENT_3D('',#3855,#3069,#3070);
#2631=AXIS2_PLACEMENT_3D('',#3857,#3071,#3072);
#2632=AXIS2_PLACEMENT_3D('',#3859,#3073,#3074);
#2633=AXIS2_PLACEMENT_3D('',#3861,#3076,#3077);
#2634=AXIS2_PLACEMENT_3D('',#3867,#3081,#3082);
#2635=AXIS2_PLACEMENT_3D('',#3868,#3083,#3084);
#2636=AXIS2_PLACEMENT_3D('',#3869,#3085,#3086);
#2637=AXIS2_PLACEMENT_3D('',#3870,#3087,#3088);
#2638=AXIS2_PLACEMENT_3D('',#3871,#3089,#3090);
#2639=AXIS2_PLACEMENT_3D('',#3872,#3091,#3092);
#2640=AXIS2_PLACEMENT_3D('',#3873,#3093,#3094);
#2641=AXIS2_PLACEMENT_3D('',#3875,#3095,#3096);
#2642=AXIS2_PLACEMENT_3D('',#3878,#3098,#3099);
#2643=AXIS2_PLACEMENT_3D('',#3879,#3100,#3101);
#2644=AXIS2_PLACEMENT_3D('',#3881,#3102,#3103);
#2645=AXIS2_PLACEMENT_3D('',#3884,#3105,#3106);
#2646=AXIS2_PLACEMENT_3D('',#3885,#3107,#3108);
#2647=AXIS2_PLACEMENT_3D('',#3894,#3113,#3114);
#2648=AXIS2_PLACEMENT_3D('',#3896,#3115,#3116);
#2649=AXIS2_PLACEMENT_3D('',#3898,#3117,#3118);
#2650=AXIS2_PLACEMENT_3D('',#3900,#3120,#3121);
#2651=AXIS2_PLACEMENT_3D('',#3906,#3125,#3126);
#2652=AXIS2_PLACEMENT_3D('',#3907,#3127,#3128);
#2653=AXIS2_PLACEMENT_3D('',#3908,#3129,#3130);
#2654=AXIS2_PLACEMENT_3D('',#3909,#3131,#3132);
#2655=AXIS2_PLACEMENT_3D('',#3910,#3133,#3134);
#2656=AXIS2_PLACEMENT_3D('',#3911,#3135,#3136);
#2657=AXIS2_PLACEMENT_3D('',#3912,#3137,#3138);
#2658=AXIS2_PLACEMENT_3D('',#3914,#3139,#3140);
#2659=AXIS2_PLACEMENT_3D('',#3917,#3142,#3143);
#2660=AXIS2_PLACEMENT_3D('',#3918,#3144,#3145);
#2661=AXIS2_PLACEMENT_3D('',#3927,#3150,#3151);
#2662=AXIS2_PLACEMENT_3D('',#3933,#3155,#3156);
#2663=AXIS2_PLACEMENT_3D('',#3939,#3160,#3161);
#2664=AXIS2_PLACEMENT_3D('',#3942,#3164,#3165);
#2665=AXIS2_PLACEMENT_3D('',#3943,#3166,#3167);
#2666=AXIS2_PLACEMENT_3D('',#3944,#3168,#3169);
#2667=AXIS2_PLACEMENT_3D('',#3945,#3170,#3171);
#2668=AXIS2_PLACEMENT_3D('',#3947,#3172,#3173);
#2669=AXIS2_PLACEMENT_3D('',#3950,#3175,#3176);
#2670=AXIS2_PLACEMENT_3D('',#3951,#3177,#3178);
#2671=AXIS2_PLACEMENT_3D('',#3953,#3179,#3180);
#2672=AXIS2_PLACEMENT_3D('',#3956,#3182,#3183);
#2673=AXIS2_PLACEMENT_3D('',#3957,#3184,#3185);
#2674=AXIS2_PLACEMENT_3D('',#3959,#3186,#3187);
#2675=AXIS2_PLACEMENT_3D('',#3962,#3189,#3190);
#2676=AXIS2_PLACEMENT_3D('',#3963,#3191,#3192);
#2677=AXIS2_PLACEMENT_3D('',#3972,#3197,#3198);
#2678=AXIS2_PLACEMENT_3D('',#3978,#3202,#3203);
#2679=AXIS2_PLACEMENT_3D('',#3984,#3207,#3208);
#2680=AXIS2_PLACEMENT_3D('',#3987,#3211,#3212);
#2681=AXIS2_PLACEMENT_3D('',#3988,#3213,#3214);
#2682=AXIS2_PLACEMENT_3D('',#3989,#3215,#3216);
#2683=AXIS2_PLACEMENT_3D('',#3990,#3217,#3218);
#2684=AXIS2_PLACEMENT_3D('',#3992,#3219,#3220);
#2685=AXIS2_PLACEMENT_3D('',#3995,#3222,#3223);
#2686=AXIS2_PLACEMENT_3D('',#3996,#3224,#3225);
#2687=AXIS2_PLACEMENT_3D('',#3998,#3226,#3227);
#2688=AXIS2_PLACEMENT_3D('',#4001,#3229,#3230);
#2689=AXIS2_PLACEMENT_3D('',#4002,#3231,#3232);
#2690=AXIS2_PLACEMENT_3D('',#4003,#3233,#3234);
#2691=AXIS2_PLACEMENT_3D('',#4004,#3235,#3236);
#2692=AXIS2_PLACEMENT_3D('',#4005,#3237,#3238);
#2693=AXIS2_PLACEMENT_3D('',#4007,#3239,#3240);
#2694=AXIS2_PLACEMENT_3D('',#4010,#3242,#3243);
#2695=AXIS2_PLACEMENT_3D('',#4011,#3244,#3245);
#2696=AXIS2_PLACEMENT_3D('',#4020,#3250,#3251);
#2697=AXIS2_PLACEMENT_3D('',#4026,#3255,#3256);
#2698=AXIS2_PLACEMENT_3D('',#4032,#3260,#3261);
#2699=AXIS2_PLACEMENT_3D('',#4035,#3264,#3265);
#2700=AXIS2_PLACEMENT_3D('',#4036,#3266,#3267);
#2701=AXIS2_PLACEMENT_3D('',#4037,#3268,#3269);
#2702=AXIS2_PLACEMENT_3D('',#4038,#3270,#3271);
#2703=AXIS2_PLACEMENT_3D('',#4040,#3272,#3273);
#2704=AXIS2_PLACEMENT_3D('',#4043,#3275,#3276);
#2705=AXIS2_PLACEMENT_3D('',#4044,#3277,#3278);
#2706=AXIS2_PLACEMENT_3D('',#4046,#3279,#3280);
#2707=AXIS2_PLACEMENT_3D('',#4047,#3281,#3282);
#2708=AXIS2_PLACEMENT_3D('',#4049,#3283,#3284);
#2709=AXIS2_PLACEMENT_3D('',#4050,#3285,#3286);
#2710=AXIS2_PLACEMENT_3D('',#4052,#3287,#3288);
#2711=AXIS2_PLACEMENT_3D('',#4054,#3290,#3291);
#2712=AXIS2_PLACEMENT_3D('',#4056,#3292,#3293);
#2713=AXIS2_PLACEMENT_3D('',#4058,#3294,#3295);
#2714=AXIS2_PLACEMENT_3D('',#4059,#3296,#3297);
#2715=AXIS2_PLACEMENT_3D('',#4062,#3299,#3300);
#2716=AXIS2_PLACEMENT_3D('',#4063,#3301,#3302);
#2717=AXIS2_PLACEMENT_3D('',#4064,#3303,#3304);
#2718=AXIS2_PLACEMENT_3D('',#4066,#3306,#3307);
#2719=AXIS2_PLACEMENT_3D('',#4067,#3308,#3309);
#2720=AXIS2_PLACEMENT_3D('',#4068,#3310,#3311);
#2721=AXIS2_PLACEMENT_3D('',#4070,#3312,#3313);
#2722=AXIS2_PLACEMENT_3D('',#4073,#3315,#3316);
#2723=AXIS2_PLACEMENT_3D('',#4074,#3317,#3318);
#2724=AXIS2_PLACEMENT_3D('',#4076,#3319,#3320);
#2725=AXIS2_PLACEMENT_3D('',#4077,#3321,#3322);
#2726=AXIS2_PLACEMENT_3D('',#4079,#3323,#3324);
#2727=AXIS2_PLACEMENT_3D('',#4080,#3325,#3326);
#2728=AXIS2_PLACEMENT_3D('',#4082,#3327,#3328);
#2729=AXIS2_PLACEMENT_3D('',#4084,#3330,#3331);
#2730=AXIS2_PLACEMENT_3D('',#4086,#3332,#3333);
#2731=AXIS2_PLACEMENT_3D('',#4088,#3334,#3335);
#2732=AXIS2_PLACEMENT_3D('',#4089,#3336,#3337);
#2733=AXIS2_PLACEMENT_3D('',#4092,#3339,#3340);
#2734=AXIS2_PLACEMENT_3D('',#4093,#3341,#3342);
#2735=AXIS2_PLACEMENT_3D('',#4094,#3343,#3344);
#2736=AXIS2_PLACEMENT_3D('',#4096,#3346,#3347);
#2737=AXIS2_PLACEMENT_3D('',#4097,#3348,#3349);
#2738=AXIS2_PLACEMENT_3D('',#4098,#3350,#3351);
#2739=AXIS2_PLACEMENT_3D('',#4100,#3352,#3353);
#2740=AXIS2_PLACEMENT_3D('',#4103,#3355,#3356);
#2741=AXIS2_PLACEMENT_3D('',#4104,#3357,#3358);
#2742=AXIS2_PLACEMENT_3D('',#4106,#3359,#3360);
#2743=AXIS2_PLACEMENT_3D('',#4107,#3361,#3362);
#2744=AXIS2_PLACEMENT_3D('',#4109,#3363,#3364);
#2745=AXIS2_PLACEMENT_3D('',#4110,#3365,#3366);
#2746=AXIS2_PLACEMENT_3D('',#4112,#3367,#3368);
#2747=AXIS2_PLACEMENT_3D('',#4114,#3370,#3371);
#2748=AXIS2_PLACEMENT_3D('',#4116,#3372,#3373);
#2749=AXIS2_PLACEMENT_3D('',#4118,#3374,#3375);
#2750=AXIS2_PLACEMENT_3D('',#4119,#3376,#3377);
#2751=AXIS2_PLACEMENT_3D('',#4122,#3379,#3380);
#2752=AXIS2_PLACEMENT_3D('',#4123,#3381,#3382);
#2753=AXIS2_PLACEMENT_3D('',#4124,#3383,#3384);
#2754=AXIS2_PLACEMENT_3D('',#4126,#3386,#3387);
#2755=AXIS2_PLACEMENT_3D('',#4127,#3388,#3389);
#2756=AXIS2_PLACEMENT_3D('',#4128,#3390,#3391);
#2757=AXIS2_PLACEMENT_3D('',#4130,#3392,#3393);
#2758=AXIS2_PLACEMENT_3D('',#4132,#3394,#3395);
#2759=AXIS2_PLACEMENT_3D('',#4133,#3396,#3397);
#2760=AXIS2_PLACEMENT_3D('',#4135,#3398,#3399);
#2761=AXIS2_PLACEMENT_3D('',#4137,#3400,#3401);
#2762=AXIS2_PLACEMENT_3D('',#4138,#3402,#3403);
#2763=AXIS2_PLACEMENT_3D('',#4140,#3405,#3406);
#2764=AXIS2_PLACEMENT_3D('',#4143,#3408,#3409);
#2765=AXIS2_PLACEMENT_3D('',#4144,#3410,#3411);
#2766=AXIS2_PLACEMENT_3D('',#4146,#3412,#3413);
#2767=AXIS2_PLACEMENT_3D('',#4149,#3415,#3416);
#2768=AXIS2_PLACEMENT_3D('',#4150,#3417,#3418);
#2769=AXIS2_PLACEMENT_3D('',#4152,#3419,#3420);
#2770=AXIS2_PLACEMENT_3D('',#4153,#3421,#3422);
#2771=AXIS2_PLACEMENT_3D('',#4155,#3423,#3424);
#2772=AXIS2_PLACEMENT_3D('',#4156,#3425,#3426);
#2773=AXIS2_PLACEMENT_3D('',#4158,#3427,#3428);
#2774=AXIS2_PLACEMENT_3D('',#4160,#3430,#3431);
#2775=AXIS2_PLACEMENT_3D('',#4162,#3432,#3433);
#2776=AXIS2_PLACEMENT_3D('',#4163,#3434,#3435);
#2777=AXIS2_PLACEMENT_3D('',#4166,#3437,#3438);
#2778=AXIS2_PLACEMENT_3D('',#4167,#3439,#3440);
#2779=AXIS2_PLACEMENT_3D('',#4168,#3441,#3442);
#2780=AXIS2_PLACEMENT_3D('',#4170,#3444,#3445);
#2781=AXIS2_PLACEMENT_3D('',#4171,#3446,#3447);
#2782=AXIS2_PLACEMENT_3D('',#4172,#3448,#3449);
#2783=AXIS2_PLACEMENT_3D('',#4174,#3450,#3451);
#2784=AXIS2_PLACEMENT_3D('',#4177,#3453,#3454);
#2785=AXIS2_PLACEMENT_3D('',#4178,#3455,#3456);
#2786=AXIS2_PLACEMENT_3D('',#4180,#3457,#3458);
#2787=AXIS2_PLACEMENT_3D('',#4181,#3459,#3460);
#2788=AXIS2_PLACEMENT_3D('',#4183,#3461,#3462);
#2789=AXIS2_PLACEMENT_3D('',#4184,#3463,#3464);
#2790=AXIS2_PLACEMENT_3D('',#4186,#3465,#3466);
#2791=AXIS2_PLACEMENT_3D('',#4188,#3468,#3469);
#2792=AXIS2_PLACEMENT_3D('',#4190,#3470,#3471);
#2793=AXIS2_PLACEMENT_3D('',#4192,#3472,#3473);
#2794=AXIS2_PLACEMENT_3D('',#4193,#3474,#3475);
#2795=AXIS2_PLACEMENT_3D('',#4196,#3477,#3478);
#2796=AXIS2_PLACEMENT_3D('',#4197,#3479,#3480);
#2797=AXIS2_PLACEMENT_3D('',#4198,#3481,#3482);
#2798=AXIS2_PLACEMENT_3D('',#4200,#3484,#3485);
#2799=AXIS2_PLACEMENT_3D('',#4201,#3486,#3487);
#2800=AXIS2_PLACEMENT_3D('',#4202,#3488,#3489);
#2801=AXIS2_PLACEMENT_3D('',#4204,#3490,#3491);
#2802=AXIS2_PLACEMENT_3D('',#4207,#3493,#3494);
#2803=AXIS2_PLACEMENT_3D('',#4208,#3495,#3496);
#2804=AXIS2_PLACEMENT_3D('',#4210,#3497,#3498);
#2805=AXIS2_PLACEMENT_3D('',#4211,#3499,#3500);
#2806=AXIS2_PLACEMENT_3D('',#4213,#3501,#3502);
#2807=AXIS2_PLACEMENT_3D('',#4214,#3503,#3504);
#2808=AXIS2_PLACEMENT_3D('',#4216,#3505,#3506);
#2809=AXIS2_PLACEMENT_3D('',#4218,#3508,#3509);
#2810=AXIS2_PLACEMENT_3D('',#4220,#3510,#3511);
#2811=AXIS2_PLACEMENT_3D('',#4222,#3512,#3513);
#2812=AXIS2_PLACEMENT_3D('',#4223,#3514,#3515);
#2813=AXIS2_PLACEMENT_3D('',#4226,#3517,#3518);
#2814=AXIS2_PLACEMENT_3D('',#4227,#3519,#3520);
#2815=AXIS2_PLACEMENT_3D('',#4228,#3521,#3522);
#2816=AXIS2_PLACEMENT_3D('',#4230,#3524,#3525);
#2817=AXIS2_PLACEMENT_3D('',#4231,#3526,#3527);
#2818=AXIS2_PLACEMENT_3D('',#4232,#3528,#3529);
#2819=AXIS2_PLACEMENT_3D('',#4234,#3530,#3531);
#2820=AXIS2_PLACEMENT_3D('',#4237,#3533,#3534);
#2821=AXIS2_PLACEMENT_3D('',#4238,#3535,#3536);
#2822=AXIS2_PLACEMENT_3D('',#4240,#3537,#3538);
#2823=AXIS2_PLACEMENT_3D('',#4243,#3540,#3541);
#2824=AXIS2_PLACEMENT_3D('',#4244,#3542,#3543);
#2825=AXIS2_PLACEMENT_3D('',#4245,#3544,#3545);
#2826=AXIS2_PLACEMENT_3D('',#4246,#3546,#3547);
#2827=AXIS2_PLACEMENT_3D('',#4247,#3548,#3549);
#2828=AXIS2_PLACEMENT_3D('',#4249,#3550,#3551);
#2829=AXIS2_PLACEMENT_3D('',#4252,#3553,#3554);
#2830=AXIS2_PLACEMENT_3D('',#4253,#3555,#3556);
#2831=AXIS2_PLACEMENT_3D('',#4255,#3557,#3558);
#2832=AXIS2_PLACEMENT_3D('',#4258,#3560,#3561);
#2833=AXIS2_PLACEMENT_3D('',#4259,#3562,#3563);
#2834=AXIS2_PLACEMENT_3D('',#4260,#3564,#3565);
#2835=AXIS2_PLACEMENT_3D('',#4261,#3566,#3567);
#2836=AXIS2_PLACEMENT_3D('',#4262,#3568,#3569);
#2837=AXIS2_PLACEMENT_3D('',#4264,#3570,#3571);
#2838=AXIS2_PLACEMENT_3D('',#4267,#3573,#3574);
#2839=AXIS2_PLACEMENT_3D('',#4268,#3575,#3576);
#2840=AXIS2_PLACEMENT_3D('',#4270,#3577,#3578);
#2841=AXIS2_PLACEMENT_3D('',#4273,#3580,#3581);
#2842=AXIS2_PLACEMENT_3D('',#4274,#3582,#3583);
#2843=AXIS2_PLACEMENT_3D('',#4275,#3584,#3585);
#2844=AXIS2_PLACEMENT_3D('',#4276,#3586,#3587);
#2845=AXIS2_PLACEMENT_3D('',#4277,#3588,#3589);
#2846=AXIS2_PLACEMENT_3D('',#4286,#3594,#3595);
#2847=AXIS2_PLACEMENT_3D('',#4295,#3600,#3601);
#2848=AXIS2_PLACEMENT_3D('',#4296,#3602,#3603);
#2849=AXIS2_PLACEMENT_3D('',#4297,#3604,#3605);
#2850=AXIS2_PLACEMENT_3D('',#4298,#3606,#3607);
#2851=AXIS2_PLACEMENT_3D('',#4299,#3608,#3609);
#2852=AXIS2_PLACEMENT_3D('',#4300,#3610,#3611);
#2853=AXIS2_PLACEMENT_3D('',#4301,#3612,#3613);
#2854=AXIS2_PLACEMENT_3D('',#4302,#3614,#3615);
#2855=AXIS2_PLACEMENT_3D('',#4303,#3616,#3617);
#2856=AXIS2_PLACEMENT_3D('',#4304,#3618,#3619);
#2857=AXIS2_PLACEMENT_3D('',#4305,#3620,#3621);
#2858=AXIS2_PLACEMENT_3D('',#4306,#3622,#3623);
#2859=AXIS2_PLACEMENT_3D('',#4307,#3624,#3625);
#2860=AXIS2_PLACEMENT_3D('',#4308,#3626,#3627);
#2861=AXIS2_PLACEMENT_3D('',#4309,#3628,#3629);
#2862=AXIS2_PLACEMENT_3D('',#4310,#3630,#3631);
#2863=AXIS2_PLACEMENT_3D('',#4311,#3632,#3633);
#2864=AXIS2_PLACEMENT_3D('',#4312,#3634,#3635);
#2865=AXIS2_PLACEMENT_3D('',#4313,#3636,#3637);
#2866=AXIS2_PLACEMENT_3D('',#4314,#3638,#3639);
#2867=AXIS2_PLACEMENT_3D('',#4315,#3640,#3641);
#2868=AXIS2_PLACEMENT_3D('',#4316,#3642,#3643);
#2869=AXIS2_PLACEMENT_3D('',#4317,#3644,#3645);
#2870=AXIS2_PLACEMENT_3D('',#4318,#3646,#3647);
#2871=AXIS2_PLACEMENT_3D('',#4319,#3648,#3649);
#2872=AXIS2_PLACEMENT_3D('',#4320,#3650,#3651);
#2873=AXIS2_PLACEMENT_3D('',#4321,#3652,#3653);
#2874=AXIS2_PLACEMENT_3D('',#4322,#3654,#3655);
#2875=AXIS2_PLACEMENT_3D('',#4323,#3656,#3657);
#2876=AXIS2_PLACEMENT_3D('',#4324,#3658,#3659);
#2877=AXIS2_PLACEMENT_3D('',#4325,#3660,#3661);
#2878=AXIS2_PLACEMENT_3D('',#4326,#3662,#3663);
#2879=AXIS2_PLACEMENT_3D('',#4327,#3664,#3665);
#2880=AXIS2_PLACEMENT_3D('',#4328,#3666,#3667);
#2881=AXIS2_PLACEMENT_3D('',#4329,#3668,#3669);
#2882=AXIS2_PLACEMENT_3D('',#4330,#3670,#3671);
#2883=AXIS2_PLACEMENT_3D('',#4331,#3672,#3673);
#2884=AXIS2_PLACEMENT_3D('',#4332,#3674,#3675);
#2885=AXIS2_PLACEMENT_3D('',#4333,#3676,#3677);
#2886=AXIS2_PLACEMENT_3D('',#4334,#3678,#3679);
#2887=AXIS2_PLACEMENT_3D('',#4335,#3680,#3681);
#2888=AXIS2_PLACEMENT_3D('',#4336,#3682,#3683);
#2889=AXIS2_PLACEMENT_3D('',#4337,#3684,#3685);
#2890=AXIS2_PLACEMENT_3D('',#4338,#3686,#3687);
#2891=AXIS2_PLACEMENT_3D('',#4339,#3688,#3689);
#2892=AXIS2_PLACEMENT_3D('',#4340,#3690,#3691);
#2893=AXIS2_PLACEMENT_3D('',#4341,#3692,#3693);
#2894=AXIS2_PLACEMENT_3D('',#4342,#3694,#3695);
#2895=AXIS2_PLACEMENT_3D('',#4343,#3696,#3697);
#2896=AXIS2_PLACEMENT_3D('',#4344,#3698,#3699);
#2897=DIRECTION('axis',(0.,0.,1.));
#2898=DIRECTION('refdir',(1.,0.,0.));
#2899=DIRECTION('axis',(0.,0.,1.));
#2900=DIRECTION('refdir',(1.,0.,0.));
#2901=DIRECTION('center_axis',(0.,0.,-1.));
#2902=DIRECTION('ref_axis',(1.,0.,0.));
#2903=DIRECTION('center_axis',(0.,0.,-1.));
#2904=DIRECTION('ref_axis',(1.,0.,0.));
#2905=DIRECTION('',(0.,0.,-1.));
#2906=DIRECTION('center_axis',(0.,0.,1.));
#2907=DIRECTION('ref_axis',(1.,0.,0.));
#2908=DIRECTION('center_axis',(0.,0.,-1.));
#2909=DIRECTION('ref_axis',(1.,0.,0.));
#2910=DIRECTION('center_axis',(0.,0.,-1.));
#2911=DIRECTION('ref_axis',(1.,0.,0.));
#2912=DIRECTION('',(0.,0.,-1.));
#2913=DIRECTION('center_axis',(0.,0.,1.));
#2914=DIRECTION('ref_axis',(1.,0.,0.));
#2915=DIRECTION('center_axis',(0.,1.,0.));
#2916=DIRECTION('ref_axis',(-1.,0.,0.));
#2917=DIRECTION('',(1.,0.,0.));
#2918=DIRECTION('',(0.,0.,1.));
#2919=DIRECTION('',(1.,0.,0.));
#2920=DIRECTION('',(0.,0.,-1.));
#2921=DIRECTION('center_axis',(1.,0.,0.));
#2922=DIRECTION('ref_axis',(0.,1.,0.));
#2923=DIRECTION('',(0.,-1.,0.));
#2924=DIRECTION('',(0.,-1.,0.));
#2925=DIRECTION('',(0.,0.,-1.));
#2926=DIRECTION('center_axis',(0.,-1.,0.));
#2927=DIRECTION('ref_axis',(1.,0.,0.));
#2928=DIRECTION('',(-1.,0.,0.));
#2929=DIRECTION('',(-1.,0.,0.));
#2930=DIRECTION('',(0.,0.,1.));
#2931=DIRECTION('center_axis',(-1.,0.,0.));
#2932=DIRECTION('ref_axis',(0.,-1.,0.));
#2933=DIRECTION('',(0.,1.,0.));
#2934=DIRECTION('',(0.,1.,0.));
#2935=DIRECTION('center_axis',(0.,0.,1.));
#2936=DIRECTION('ref_axis',(1.,0.,0.));
#2937=DIRECTION('center_axis',(0.,0.,1.));
#2938=DIRECTION('ref_axis',(1.,0.,0.));
#2939=DIRECTION('axis',(0.,0.,1.));
#2940=DIRECTION('refdir',(1.,0.,0.));
#2941=DIRECTION('center_axis',(0.,0.,1.));
#2942=DIRECTION('ref_axis',(1.,0.,0.));
#2943=DIRECTION('center_axis',(0.,0.,-1.));
#2944=DIRECTION('ref_axis',(1.,0.,0.));
#2945=DIRECTION('',(0.,0.,-1.));
#2946=DIRECTION('center_axis',(0.,0.,-1.));
#2947=DIRECTION('ref_axis',(1.,0.,0.));
#2948=DIRECTION('center_axis',(0.,0.,1.));
#2949=DIRECTION('ref_axis',(1.,0.,0.));
#2950=DIRECTION('center_axis',(0.,0.,1.));
#2951=DIRECTION('ref_axis',(1.,0.,0.));
#2952=DIRECTION('',(0.,0.,-1.));
#2953=DIRECTION('center_axis',(0.,0.,1.));
#2954=DIRECTION('ref_axis',(1.,0.,0.));
#2955=DIRECTION('center_axis',(0.,0.,1.));
#2956=DIRECTION('ref_axis',(1.,0.,0.));
#2957=DIRECTION('center_axis',(0.,0.,1.));
#2958=DIRECTION('ref_axis',(1.,0.,0.));
#2959=DIRECTION('axis',(0.,0.,1.));
#2960=DIRECTION('refdir',(1.,0.,0.));
#2961=DIRECTION('center_axis',(0.,0.,1.));
#2962=DIRECTION('ref_axis',(1.,0.,0.));
#2963=DIRECTION('center_axis',(0.,0.,-1.));
#2964=DIRECTION('ref_axis',(1.,0.,0.));
#2965=DIRECTION('',(0.,0.,-1.));
#2966=DIRECTION('center_axis',(0.,0.,-1.));
#2967=DIRECTION('ref_axis',(1.,0.,0.));
#2968=DIRECTION('center_axis',(0.,0.,1.));
#2969=DIRECTION('ref_axis',(1.,0.,0.));
#2970=DIRECTION('center_axis',(0.,0.,1.));
#2971=DIRECTION('ref_axis',(1.,0.,0.));
#2972=DIRECTION('',(0.,0.,-1.));
#2973=DIRECTION('center_axis',(0.,0.,1.));
#2974=DIRECTION('ref_axis',(1.,0.,0.));
#2975=DIRECTION('center_axis',(0.,0.,1.));
#2976=DIRECTION('ref_axis',(1.,0.,0.));
#2977=DIRECTION('center_axis',(0.,0.,1.));
#2978=DIRECTION('ref_axis',(1.,0.,0.));
#2979=DIRECTION('axis',(0.,0.,1.));
#2980=DIRECTION('refdir',(1.,0.,0.));
#2981=DIRECTION('center_axis',(0.,0.,-1.));
#2982=DIRECTION('ref_axis',(1.,0.,0.));
#2983=DIRECTION('center_axis',(0.,0.,-1.));
#2984=DIRECTION('ref_axis',(1.,0.,0.));
#2985=DIRECTION('',(0.,0.,-1.));
#2986=DIRECTION('center_axis',(0.,0.,1.));
#2987=DIRECTION('ref_axis',(1.,0.,0.));
#2988=DIRECTION('center_axis',(0.,0.,-1.));
#2989=DIRECTION('ref_axis',(1.,0.,0.));
#2990=DIRECTION('center_axis',(0.,0.,-1.));
#2991=DIRECTION('ref_axis',(1.,0.,0.));
#2992=DIRECTION('',(0.,0.,-1.));
#2993=DIRECTION('center_axis',(0.,0.,1.));
#2994=DIRECTION('ref_axis',(1.,0.,0.));
#2995=DIRECTION('center_axis',(0.,1.,0.));
#2996=DIRECTION('ref_axis',(-1.,0.,0.));
#2997=DIRECTION('',(-1.,0.,0.));
#2998=DIRECTION('',(0.,0.,1.));
#2999=DIRECTION('',(-1.,0.,0.));
#3000=DIRECTION('',(0.,0.,1.));
#3001=DIRECTION('center_axis',(0.,0.,1.));
#3002=DIRECTION('ref_axis',(0.,-1.,0.));
#3003=DIRECTION('center_axis',(0.,0.,1.));
#3004=DIRECTION('ref_axis',(0.,-1.,0.));
#3005=DIRECTION('center_axis',(0.,0.,1.));
#3006=DIRECTION('ref_axis',(0.,-1.,0.));
#3007=DIRECTION('',(0.,0.,1.));
#3008=DIRECTION('center_axis',(0.,-1.,0.));
#3009=DIRECTION('ref_axis',(1.,0.,0.));
#3010=DIRECTION('',(1.,0.,0.));
#3011=DIRECTION('',(1.,0.,0.));
#3012=DIRECTION('',(0.,0.,1.));
#3013=DIRECTION('center_axis',(0.,0.,1.));
#3014=DIRECTION('ref_axis',(0.,1.,0.));
#3015=DIRECTION('center_axis',(0.,0.,1.));
#3016=DIRECTION('ref_axis',(0.,1.,0.));
#3017=DIRECTION('center_axis',(0.,0.,1.));
#3018=DIRECTION('ref_axis',(0.,1.,0.));
#3019=DIRECTION('center_axis',(0.,0.,1.));
#3020=DIRECTION('ref_axis',(1.,0.,0.));
#3021=DIRECTION('center_axis',(0.,0.,1.));
#3022=DIRECTION('ref_axis',(1.,0.,0.));
#3023=DIRECTION('axis',(0.,0.,1.));
#3024=DIRECTION('refdir',(1.,0.,0.));
#3025=DIRECTION('center_axis',(0.,-1.,0.));
#3026=DIRECTION('ref_axis',(-1.,0.,0.));
#3027=DIRECTION('',(-1.,0.,0.));
#3028=DIRECTION('',(0.,0.,-1.));
#3029=DIRECTION('',(1.,0.,0.));
#3030=DIRECTION('',(0.,0.,-1.));
#3031=DIRECTION('center_axis',(0.,0.,-1.));
#3032=DIRECTION('ref_axis',(0.,-1.,0.));
#3033=DIRECTION('center_axis',(0.,0.,-1.));
#3034=DIRECTION('ref_axis',(0.,-1.,0.));
#3035=DIRECTION('',(0.,0.,-1.));
#3036=DIRECTION('center_axis',(0.,0.,1.));
#3037=DIRECTION('ref_axis',(0.,-1.,0.));
#3038=DIRECTION('center_axis',(0.,1.,0.));
#3039=DIRECTION('ref_axis',(1.,0.,0.));
#3040=DIRECTION('',(1.,0.,0.));
#3041=DIRECTION('',(0.,0.,-1.));
#3042=DIRECTION('',(-1.,0.,0.));
#3043=DIRECTION('center_axis',(0.,0.,-1.));
#3044=DIRECTION('ref_axis',(0.,1.,0.));
#3045=DIRECTION('center_axis',(0.,0.,-1.));
#3046=DIRECTION('ref_axis',(0.,1.,0.));
#3047=DIRECTION('center_axis',(0.,0.,1.));
#3048=DIRECTION('ref_axis',(0.,1.,0.));
#3049=DIRECTION('center_axis',(0.,0.,-1.));
#3050=DIRECTION('ref_axis',(1.,0.,0.));
#3051=DIRECTION('center_axis',(0.,0.,-1.));
#3052=DIRECTION('ref_axis',(1.,0.,0.));
#3053=DIRECTION('',(0.,0.,-1.));
#3054=DIRECTION('center_axis',(0.,0.,1.));
#3055=DIRECTION('ref_axis',(1.,0.,0.));
#3056=DIRECTION('center_axis',(0.,0.,-1.));
#3057=DIRECTION('ref_axis',(1.,0.,0.));
#3058=DIRECTION('center_axis',(0.,0.,-1.));
#3059=DIRECTION('ref_axis',(1.,0.,0.));
#3060=DIRECTION('',(0.,0.,-1.));
#3061=DIRECTION('center_axis',(0.,0.,1.));
#3062=DIRECTION('ref_axis',(1.,0.,0.));
#3063=DIRECTION('center_axis',(0.,1.,0.));
#3064=DIRECTION('ref_axis',(-1.,0.,0.));
#3065=DIRECTION('',(-1.,0.,0.));
#3066=DIRECTION('',(0.,0.,1.));
#3067=DIRECTION('',(-1.,0.,0.));
#3068=DIRECTION('',(0.,0.,1.));
#3069=DIRECTION('center_axis',(0.,0.,1.));
#3070=DIRECTION('ref_axis',(0.,-1.,0.));
#3071=DIRECTION('center_axis',(0.,0.,1.));
#3072=DIRECTION('ref_axis',(0.,-1.,0.));
#3073=DIRECTION('center_axis',(0.,0.,1.));
#3074=DIRECTION('ref_axis',(0.,-1.,0.));
#3075=DIRECTION('',(0.,0.,1.));
#3076=DIRECTION('center_axis',(0.,-1.,0.));
#3077=DIRECTION('ref_axis',(1.,0.,0.));
#3078=DIRECTION('',(1.,0.,0.));
#3079=DIRECTION('',(1.,0.,0.));
#3080=DIRECTION('',(0.,0.,1.));
#3081=DIRECTION('center_axis',(0.,0.,1.));
#3082=DIRECTION('ref_axis',(0.,1.,0.));
#3083=DIRECTION('center_axis',(0.,0.,1.));
#3084=DIRECTION('ref_axis',(0.,1.,0.));
#3085=DIRECTION('center_axis',(0.,0.,1.));
#3086=DIRECTION('ref_axis',(0.,1.,0.));
#3087=DIRECTION('center_axis',(0.,0.,1.));
#3088=DIRECTION('ref_axis',(1.,0.,0.));
#3089=DIRECTION('center_axis',(0.,0.,1.));
#3090=DIRECTION('ref_axis',(1.,0.,0.));
#3091=DIRECTION('axis',(0.,0.,1.));
#3092=DIRECTION('refdir',(1.,0.,0.));
#3093=DIRECTION('center_axis',(0.,0.,-1.));
#3094=DIRECTION('ref_axis',(1.,0.,0.));
#3095=DIRECTION('center_axis',(0.,0.,-1.));
#3096=DIRECTION('ref_axis',(1.,0.,0.));
#3097=DIRECTION('',(0.,0.,-1.));
#3098=DIRECTION('center_axis',(0.,0.,1.));
#3099=DIRECTION('ref_axis',(1.,0.,0.));
#3100=DIRECTION('center_axis',(0.,0.,-1.));
#3101=DIRECTION('ref_axis',(1.,0.,0.));
#3102=DIRECTION('center_axis',(0.,0.,-1.));
#3103=DIRECTION('ref_axis',(1.,0.,0.));
#3104=DIRECTION('',(0.,0.,-1.));
#3105=DIRECTION('center_axis',(0.,0.,1.));
#3106=DIRECTION('ref_axis',(1.,0.,0.));
#3107=DIRECTION('center_axis',(0.,1.,0.));
#3108=DIRECTION('ref_axis',(-1.,0.,0.));
#3109=DIRECTION('',(-1.,0.,0.));
#3110=DIRECTION('',(0.,0.,1.));
#3111=DIRECTION('',(-1.,0.,0.));
#3112=DIRECTION('',(0.,0.,1.));
#3113=DIRECTION('center_axis',(0.,0.,1.));
#3114=DIRECTION('ref_axis',(0.,-1.,0.));
#3115=DIRECTION('center_axis',(0.,0.,1.));
#3116=DIRECTION('ref_axis',(0.,-1.,0.));
#3117=DIRECTION('center_axis',(0.,0.,1.));
#3118=DIRECTION('ref_axis',(0.,-1.,0.));
#3119=DIRECTION('',(0.,0.,1.));
#3120=DIRECTION('center_axis',(0.,-1.,0.));
#3121=DIRECTION('ref_axis',(1.,0.,0.));
#3122=DIRECTION('',(1.,0.,0.));
#3123=DIRECTION('',(1.,0.,0.));
#3124=DIRECTION('',(0.,0.,1.));
#3125=DIRECTION('center_axis',(0.,0.,1.));
#3126=DIRECTION('ref_axis',(0.,1.,0.));
#3127=DIRECTION('center_axis',(0.,0.,1.));
#3128=DIRECTION('ref_axis',(0.,1.,0.));
#3129=DIRECTION('center_axis',(0.,0.,1.));
#3130=DIRECTION('ref_axis',(0.,1.,0.));
#3131=DIRECTION('center_axis',(0.,0.,1.));
#3132=DIRECTION('ref_axis',(1.,0.,0.));
#3133=DIRECTION('center_axis',(0.,0.,1.));
#3134=DIRECTION('ref_axis',(1.,0.,0.));
#3135=DIRECTION('axis',(0.,0.,1.));
#3136=DIRECTION('refdir',(1.,0.,0.));
#3137=DIRECTION('center_axis',(0.,0.,-1.));
#3138=DIRECTION('ref_axis',(1.,0.,0.));
#3139=DIRECTION('center_axis',(0.,0.,-1.));
#3140=DIRECTION('ref_axis',(1.,0.,0.));
#3141=DIRECTION('',(0.,0.,-1.));
#3142=DIRECTION('center_axis',(0.,0.,1.));
#3143=DIRECTION('ref_axis',(1.,0.,0.));
#3144=DIRECTION('center_axis',(0.,1.,0.));
#3145=DIRECTION('ref_axis',(-1.,0.,0.));
#3146=DIRECTION('',(-1.,0.,0.));
#3147=DIRECTION('',(0.,0.,1.));
#3148=DIRECTION('',(-1.,0.,0.));
#3149=DIRECTION('',(0.,0.,1.));
#3150=DIRECTION('center_axis',(1.,0.,0.));
#3151=DIRECTION('ref_axis',(0.,1.,0.));
#3152=DIRECTION('',(0.,1.,0.));
#3153=DIRECTION('',(0.,1.,0.));
#3154=DIRECTION('',(0.,0.,1.));
#3155=DIRECTION('center_axis',(0.,-1.,0.));
#3156=DIRECTION('ref_axis',(1.,0.,0.));
#3157=DIRECTION('',(1.,0.,0.));
#3158=DIRECTION('',(1.,0.,0.));
#3159=DIRECTION('',(0.,0.,1.));
#3160=DIRECTION('center_axis',(-1.,0.,0.));
#3161=DIRECTION('ref_axis',(0.,-1.,0.));
#3162=DIRECTION('',(0.,-1.,0.));
#3163=DIRECTION('',(0.,-1.,0.));
#3164=DIRECTION('center_axis',(0.,0.,1.));
#3165=DIRECTION('ref_axis',(1.,0.,0.));
#3166=DIRECTION('center_axis',(0.,0.,1.));
#3167=DIRECTION('ref_axis',(1.,0.,0.));
#3168=DIRECTION('axis',(0.,0.,1.));
#3169=DIRECTION('refdir',(1.,0.,0.));
#3170=DIRECTION('center_axis',(0.,0.,-1.));
#3171=DIRECTION('ref_axis',(1.,0.,0.));
#3172=DIRECTION('center_axis',(0.,0.,-1.));
#3173=DIRECTION('ref_axis',(1.,0.,0.));
#3174=DIRECTION('',(0.,0.,-1.));
#3175=DIRECTION('center_axis',(0.,0.,1.));
#3176=DIRECTION('ref_axis',(1.,0.,0.));
#3177=DIRECTION('center_axis',(0.,-1.,0.));
#3178=DIRECTION('ref_axis',(0.,0.,1.));
#3179=DIRECTION('center_axis',(0.,-1.,0.));
#3180=DIRECTION('ref_axis',(0.,0.,1.));
#3181=DIRECTION('',(0.,-1.,0.));
#3182=DIRECTION('center_axis',(0.,1.,0.));
#3183=DIRECTION('ref_axis',(0.,0.,1.));
#3184=DIRECTION('center_axis',(0.,-1.,0.));
#3185=DIRECTION('ref_axis',(0.,0.,1.));
#3186=DIRECTION('center_axis',(0.,-1.,0.));
#3187=DIRECTION('ref_axis',(0.,0.,1.));
#3188=DIRECTION('',(0.,-1.,0.));
#3189=DIRECTION('center_axis',(0.,1.,0.));
#3190=DIRECTION('ref_axis',(0.,0.,1.));
#3191=DIRECTION('center_axis',(0.,1.,0.));
#3192=DIRECTION('ref_axis',(-1.,0.,0.));
#3193=DIRECTION('',(-1.,0.,0.));
#3194=DIRECTION('',(0.,0.,1.));
#3195=DIRECTION('',(-1.,0.,0.));
#3196=DIRECTION('',(0.,0.,1.));
#3197=DIRECTION('center_axis',(1.,0.,0.));
#3198=DIRECTION('ref_axis',(0.,1.,0.));
#3199=DIRECTION('',(0.,1.,0.));
#3200=DIRECTION('',(0.,1.,0.));
#3201=DIRECTION('',(0.,0.,1.));
#3202=DIRECTION('center_axis',(0.,-1.,0.));
#3203=DIRECTION('ref_axis',(1.,0.,0.));
#3204=DIRECTION('',(1.,0.,0.));
#3205=DIRECTION('',(1.,0.,0.));
#3206=DIRECTION('',(0.,0.,1.));
#3207=DIRECTION('center_axis',(-1.,0.,0.));
#3208=DIRECTION('ref_axis',(0.,-1.,0.));
#3209=DIRECTION('',(0.,-1.,0.));
#3210=DIRECTION('',(0.,-1.,0.));
#3211=DIRECTION('center_axis',(0.,0.,1.));
#3212=DIRECTION('ref_axis',(1.,0.,0.));
#3213=DIRECTION('center_axis',(0.,0.,1.));
#3214=DIRECTION('ref_axis',(1.,0.,0.));
#3215=DIRECTION('axis',(0.,0.,1.));
#3216=DIRECTION('refdir',(1.,0.,0.));
#3217=DIRECTION('center_axis',(0.,0.,1.));
#3218=DIRECTION('ref_axis',(1.,0.,0.));
#3219=DIRECTION('center_axis',(0.,0.,-1.));
#3220=DIRECTION('ref_axis',(1.,0.,0.));
#3221=DIRECTION('',(0.,0.,-1.));
#3222=DIRECTION('center_axis',(0.,0.,-1.));
#3223=DIRECTION('ref_axis',(1.,0.,0.));
#3224=DIRECTION('center_axis',(0.,0.,1.));
#3225=DIRECTION('ref_axis',(1.,0.,0.));
#3226=DIRECTION('center_axis',(0.,0.,1.));
#3227=DIRECTION('ref_axis',(1.,0.,0.));
#3228=DIRECTION('',(0.,0.,-1.));
#3229=DIRECTION('center_axis',(0.,0.,1.));
#3230=DIRECTION('ref_axis',(1.,0.,0.));
#3231=DIRECTION('center_axis',(0.,0.,1.));
#3232=DIRECTION('ref_axis',(1.,0.,0.));
#3233=DIRECTION('center_axis',(0.,0.,1.));
#3234=DIRECTION('ref_axis',(1.,0.,0.));
#3235=DIRECTION('axis',(0.,0.,1.));
#3236=DIRECTION('refdir',(1.,0.,0.));
#3237=DIRECTION('center_axis',(0.,-1.,0.));
#3238=DIRECTION('ref_axis',(0.,0.,1.));
#3239=DIRECTION('center_axis',(0.,-1.,0.));
#3240=DIRECTION('ref_axis',(0.,0.,1.));
#3241=DIRECTION('',(0.,-1.,0.));
#3242=DIRECTION('center_axis',(0.,1.,0.));
#3243=DIRECTION('ref_axis',(0.,0.,1.));
#3244=DIRECTION('center_axis',(0.,1.,0.));
#3245=DIRECTION('ref_axis',(-1.,0.,0.));
#3246=DIRECTION('',(-1.,0.,0.));
#3247=DIRECTION('',(0.,0.,1.));
#3248=DIRECTION('',(-1.,0.,0.));
#3249=DIRECTION('',(0.,0.,1.));
#3250=DIRECTION('center_axis',(1.,0.,0.));
#3251=DIRECTION('ref_axis',(0.,1.,0.));
#3252=DIRECTION('',(0.,1.,0.));
#3253=DIRECTION('',(0.,1.,0.));
#3254=DIRECTION('',(0.,0.,1.));
#3255=DIRECTION('center_axis',(0.,-1.,0.));
#3256=DIRECTION('ref_axis',(1.,0.,0.));
#3257=DIRECTION('',(1.,0.,0.));
#3258=DIRECTION('',(1.,0.,0.));
#3259=DIRECTION('',(0.,0.,1.));
#3260=DIRECTION('center_axis',(-1.,0.,0.));
#3261=DIRECTION('ref_axis',(0.,-1.,0.));
#3262=DIRECTION('',(0.,-1.,0.));
#3263=DIRECTION('',(0.,-1.,0.));
#3264=DIRECTION('center_axis',(0.,0.,1.));
#3265=DIRECTION('ref_axis',(1.,0.,0.));
#3266=DIRECTION('center_axis',(0.,0.,1.));
#3267=DIRECTION('ref_axis',(1.,0.,0.));
#3268=DIRECTION('axis',(0.,0.,1.));
#3269=DIRECTION('refdir',(1.,0.,0.));
#3270=DIRECTION('center_axis',(0.,0.,1.));
#3271=DIRECTION('ref_axis',(1.,0.,0.));
#3272=DIRECTION('center_axis',(0.,0.,1.));
#3273=DIRECTION('ref_axis',(1.,0.,0.));
#3274=DIRECTION('',(0.,0.,1.));
#3275=DIRECTION('center_axis',(0.,0.,1.));
#3276=DIRECTION('ref_axis',(1.,0.,0.));
#3277=DIRECTION('center_axis',(0.,0.,-1.));
#3278=DIRECTION('ref_axis',(-1.,0.,0.));
#3279=DIRECTION('center_axis',(0.,0.,-1.));
#3280=DIRECTION('ref_axis',(1.,0.,0.));
#3281=DIRECTION('center_axis',(0.,0.,1.));
#3282=DIRECTION('ref_axis',(1.,0.,0.));
#3283=DIRECTION('center_axis',(0.,0.,1.));
#3284=DIRECTION('ref_axis',(1.,0.,0.));
#3285=DIRECTION('center_axis',(0.,0.,1.));
#3286=DIRECTION('ref_axis',(1.,0.,0.));
#3287=DIRECTION('center_axis',(0.,0.,1.));
#3288=DIRECTION('ref_axis',(1.,0.,0.));
#3289=DIRECTION('',(0.,0.,-1.));
#3290=DIRECTION('center_axis',(0.,0.,1.));
#3291=DIRECTION('ref_axis',(1.,0.,0.));
#3292=DIRECTION('center_axis',(0.,0.,1.));
#3293=DIRECTION('ref_axis',(1.,0.,0.));
#3294=DIRECTION('center_axis',(0.,0.,1.));
#3295=DIRECTION('ref_axis',(1.,0.,0.));
#3296=DIRECTION('center_axis',(0.,0.,1.));
#3297=DIRECTION('ref_axis',(1.,0.,0.));
#3298=DIRECTION('',(0.,0.,-1.));
#3299=DIRECTION('center_axis',(0.,0.,1.));
#3300=DIRECTION('ref_axis',(1.,0.,0.));
#3301=DIRECTION('center_axis',(0.,0.,1.));
#3302=DIRECTION('ref_axis',(1.,0.,0.));
#3303=DIRECTION('center_axis',(0.,0.,1.));
#3304=DIRECTION('ref_axis',(1.,0.,0.));
#3305=DIRECTION('',(0.,0.,-1.));
#3306=DIRECTION('center_axis',(0.,0.,1.));
#3307=DIRECTION('ref_axis',(1.,0.,0.));
#3308=DIRECTION('axis',(0.,0.,1.));
#3309=DIRECTION('refdir',(1.,0.,0.));
#3310=DIRECTION('center_axis',(0.,0.,1.));
#3311=DIRECTION('ref_axis',(1.,0.,0.));
#3312=DIRECTION('center_axis',(0.,0.,1.));
#3313=DIRECTION('ref_axis',(1.,0.,0.));
#3314=DIRECTION('',(0.,0.,1.));
#3315=DIRECTION('center_axis',(0.,0.,1.));
#3316=DIRECTION('ref_axis',(1.,0.,0.));
#3317=DIRECTION('center_axis',(0.,0.,-1.));
#3318=DIRECTION('ref_axis',(-1.,0.,0.));
#3319=DIRECTION('center_axis',(0.,0.,-1.));
#3320=DIRECTION('ref_axis',(1.,0.,0.));
#3321=DIRECTION('center_axis',(0.,0.,1.));
#3322=DIRECTION('ref_axis',(1.,0.,0.));
#3323=DIRECTION('center_axis',(0.,0.,1.));
#3324=DIRECTION('ref_axis',(1.,0.,0.));
#3325=DIRECTION('center_axis',(0.,0.,1.));
#3326=DIRECTION('ref_axis',(1.,0.,0.));
#3327=DIRECTION('center_axis',(0.,0.,1.));
#3328=DIRECTION('ref_axis',(1.,0.,0.));
#3329=DIRECTION('',(0.,0.,-1.));
#3330=DIRECTION('center_axis',(0.,0.,1.));
#3331=DIRECTION('ref_axis',(1.,0.,0.));
#3332=DIRECTION('center_axis',(0.,0.,1.));
#3333=DIRECTION('ref_axis',(1.,0.,0.));
#3334=DIRECTION('center_axis',(0.,0.,1.));
#3335=DIRECTION('ref_axis',(1.,0.,0.));
#3336=DIRECTION('center_axis',(0.,0.,1.));
#3337=DIRECTION('ref_axis',(1.,0.,0.));
#3338=DIRECTION('',(0.,0.,-1.));
#3339=DIRECTION('center_axis',(0.,0.,1.));
#3340=DIRECTION('ref_axis',(1.,0.,0.));
#3341=DIRECTION('center_axis',(0.,0.,1.));
#3342=DIRECTION('ref_axis',(1.,0.,0.));
#3343=DIRECTION('center_axis',(0.,0.,1.));
#3344=DIRECTION('ref_axis',(1.,0.,0.));
#3345=DIRECTION('',(0.,0.,-1.));
#3346=DIRECTION('center_axis',(0.,0.,1.));
#3347=DIRECTION('ref_axis',(1.,0.,0.));
#3348=DIRECTION('axis',(0.,0.,1.));
#3349=DIRECTION('refdir',(1.,0.,0.));
#3350=DIRECTION('center_axis',(0.,0.,1.));
#3351=DIRECTION('ref_axis',(1.,0.,0.));
#3352=DIRECTION('center_axis',(0.,0.,1.));
#3353=DIRECTION('ref_axis',(1.,0.,0.));
#3354=DIRECTION('',(0.,0.,1.));
#3355=DIRECTION('center_axis',(0.,0.,1.));
#3356=DIRECTION('ref_axis',(1.,0.,0.));
#3357=DIRECTION('center_axis',(0.,0.,-1.));
#3358=DIRECTION('ref_axis',(-1.,0.,0.));
#3359=DIRECTION('center_axis',(0.,0.,-1.));
#3360=DIRECTION('ref_axis',(1.,0.,0.));
#3361=DIRECTION('center_axis',(0.,0.,1.));
#3362=DIRECTION('ref_axis',(1.,0.,0.));
#3363=DIRECTION('center_axis',(0.,0.,1.));
#3364=DIRECTION('ref_axis',(1.,0.,0.));
#3365=DIRECTION('center_axis',(0.,0.,1.));
#3366=DIRECTION('ref_axis',(1.,0.,0.));
#3367=DIRECTION('center_axis',(0.,0.,1.));
#3368=DIRECTION('ref_axis',(1.,0.,0.));
#3369=DIRECTION('',(0.,0.,-1.));
#3370=DIRECTION('center_axis',(0.,0.,1.));
#3371=DIRECTION('ref_axis',(1.,0.,0.));
#3372=DIRECTION('center_axis',(0.,0.,1.));
#3373=DIRECTION('ref_axis',(1.,0.,0.));
#3374=DIRECTION('center_axis',(0.,0.,1.));
#3375=DIRECTION('ref_axis',(1.,0.,0.));
#3376=DIRECTION('center_axis',(0.,0.,1.));
#3377=DIRECTION('ref_axis',(1.,0.,0.));
#3378=DIRECTION('',(0.,0.,-1.));
#3379=DIRECTION('center_axis',(0.,0.,1.));
#3380=DIRECTION('ref_axis',(1.,0.,0.));
#3381=DIRECTION('center_axis',(0.,0.,1.));
#3382=DIRECTION('ref_axis',(1.,0.,0.));
#3383=DIRECTION('center_axis',(0.,0.,1.));
#3384=DIRECTION('ref_axis',(1.,0.,0.));
#3385=DIRECTION('',(0.,0.,-1.));
#3386=DIRECTION('center_axis',(0.,0.,1.));
#3387=DIRECTION('ref_axis',(1.,0.,0.));
#3388=DIRECTION('axis',(0.,0.,1.));
#3389=DIRECTION('refdir',(1.,0.,0.));
#3390=DIRECTION('center_axis',(0.,0.,1.));
#3391=DIRECTION('ref_axis',(1.,0.,0.));
#3392=DIRECTION('center_axis',(0.,0.,1.));
#3393=DIRECTION('ref_axis',(1.,0.,0.));
#3394=DIRECTION('center_axis',(0.,0.,1.));
#3395=DIRECTION('ref_axis',(1.,0.,0.));
#3396=DIRECTION('center_axis',(0.,0.,1.));
#3397=DIRECTION('ref_axis',(1.,0.,0.));
#3398=DIRECTION('center_axis',(0.,0.,1.));
#3399=DIRECTION('ref_axis',(1.,0.,0.));
#3400=DIRECTION('center_axis',(0.,0.,-1.));
#3401=DIRECTION('ref_axis',(1.,0.,0.));
#3402=DIRECTION('center_axis',(0.,0.,1.));
#3403=DIRECTION('ref_axis',(1.,0.,0.));
#3404=DIRECTION('',(0.,0.,-1.));
#3405=DIRECTION('center_axis',(0.,0.,1.));
#3406=DIRECTION('ref_axis',(1.,0.,0.));
#3407=DIRECTION('',(0.,0.,-1.));
#3408=DIRECTION('center_axis',(0.,0.,1.));
#3409=DIRECTION('ref_axis',(1.,0.,0.));
#3410=DIRECTION('center_axis',(0.,0.,1.));
#3411=DIRECTION('ref_axis',(1.,0.,0.));
#3412=DIRECTION('center_axis',(0.,0.,1.));
#3413=DIRECTION('ref_axis',(1.,0.,0.));
#3414=DIRECTION('',(0.,0.,1.));
#3415=DIRECTION('center_axis',(0.,0.,1.));
#3416=DIRECTION('ref_axis',(1.,0.,0.));
#3417=DIRECTION('center_axis',(0.,0.,-1.));
#3418=DIRECTION('ref_axis',(-1.,0.,0.));
#3419=DIRECTION('center_axis',(0.,0.,-1.));
#3420=DIRECTION('ref_axis',(1.,0.,0.));
#3421=DIRECTION('center_axis',(0.,0.,1.));
#3422=DIRECTION('ref_axis',(1.,0.,0.));
#3423=DIRECTION('center_axis',(0.,0.,1.));
#3424=DIRECTION('ref_axis',(1.,0.,0.));
#3425=DIRECTION('center_axis',(0.,0.,1.));
#3426=DIRECTION('ref_axis',(1.,0.,0.));
#3427=DIRECTION('center_axis',(0.,0.,1.));
#3428=DIRECTION('ref_axis',(1.,0.,0.));
#3429=DIRECTION('',(0.,0.,-1.));
#3430=DIRECTION('center_axis',(0.,0.,1.));
#3431=DIRECTION('ref_axis',(1.,0.,0.));
#3432=DIRECTION('center_axis',(0.,0.,1.));
#3433=DIRECTION('ref_axis',(1.,0.,0.));
#3434=DIRECTION('center_axis',(0.,0.,1.));
#3435=DIRECTION('ref_axis',(1.,0.,0.));
#3436=DIRECTION('',(0.,0.,-1.));
#3437=DIRECTION('center_axis',(0.,0.,1.));
#3438=DIRECTION('ref_axis',(1.,0.,0.));
#3439=DIRECTION('center_axis',(0.,0.,1.));
#3440=DIRECTION('ref_axis',(1.,0.,0.));
#3441=DIRECTION('center_axis',(0.,0.,1.));
#3442=DIRECTION('ref_axis',(1.,0.,0.));
#3443=DIRECTION('',(0.,0.,-1.));
#3444=DIRECTION('center_axis',(0.,0.,1.));
#3445=DIRECTION('ref_axis',(1.,0.,0.));
#3446=DIRECTION('axis',(0.,0.,1.));
#3447=DIRECTION('refdir',(1.,0.,0.));
#3448=DIRECTION('center_axis',(0.,0.,1.));
#3449=DIRECTION('ref_axis',(1.,0.,0.));
#3450=DIRECTION('center_axis',(0.,0.,1.));
#3451=DIRECTION('ref_axis',(1.,0.,0.));
#3452=DIRECTION('',(0.,0.,1.));
#3453=DIRECTION('center_axis',(0.,0.,1.));
#3454=DIRECTION('ref_axis',(1.,0.,0.));
#3455=DIRECTION('center_axis',(0.,0.,-1.));
#3456=DIRECTION('ref_axis',(-1.,0.,0.));
#3457=DIRECTION('center_axis',(0.,0.,-1.));
#3458=DIRECTION('ref_axis',(1.,0.,0.));
#3459=DIRECTION('center_axis',(0.,0.,1.));
#3460=DIRECTION('ref_axis',(1.,0.,0.));
#3461=DIRECTION('center_axis',(0.,0.,1.));
#3462=DIRECTION('ref_axis',(1.,0.,0.));
#3463=DIRECTION('center_axis',(0.,0.,1.));
#3464=DIRECTION('ref_axis',(1.,0.,0.));
#3465=DIRECTION('center_axis',(0.,0.,1.));
#3466=DIRECTION('ref_axis',(1.,0.,0.));
#3467=DIRECTION('',(0.,0.,-1.));
#3468=DIRECTION('center_axis',(0.,0.,1.));
#3469=DIRECTION('ref_axis',(1.,0.,0.));
#3470=DIRECTION('center_axis',(0.,0.,1.));
#3471=DIRECTION('ref_axis',(1.,0.,0.));
#3472=DIRECTION('center_axis',(0.,0.,1.));
#3473=DIRECTION('ref_axis',(1.,0.,0.));
#3474=DIRECTION('center_axis',(0.,0.,1.));
#3475=DIRECTION('ref_axis',(1.,0.,0.));
#3476=DIRECTION('',(0.,0.,-1.));
#3477=DIRECTION('center_axis',(0.,0.,1.));
#3478=DIRECTION('ref_axis',(1.,0.,0.));
#3479=DIRECTION('center_axis',(0.,0.,1.));
#3480=DIRECTION('ref_axis',(1.,0.,0.));
#3481=DIRECTION('center_axis',(0.,0.,1.));
#3482=DIRECTION('ref_axis',(1.,0.,0.));
#3483=DIRECTION('',(0.,0.,-1.));
#3484=DIRECTION('center_axis',(0.,0.,1.));
#3485=DIRECTION('ref_axis',(1.,0.,0.));
#3486=DIRECTION('axis',(0.,0.,1.));
#3487=DIRECTION('refdir',(1.,0.,0.));
#3488=DIRECTION('center_axis',(0.,0.,1.));
#3489=DIRECTION('ref_axis',(1.,0.,0.));
#3490=DIRECTION('center_axis',(0.,0.,1.));
#3491=DIRECTION('ref_axis',(1.,0.,0.));
#3492=DIRECTION('',(0.,0.,1.));
#3493=DIRECTION('center_axis',(0.,0.,1.));
#3494=DIRECTION('ref_axis',(1.,0.,0.));
#3495=DIRECTION('center_axis',(0.,0.,-1.));
#3496=DIRECTION('ref_axis',(-1.,0.,0.));
#3497=DIRECTION('center_axis',(0.,0.,-1.));
#3498=DIRECTION('ref_axis',(1.,0.,0.));
#3499=DIRECTION('center_axis',(0.,0.,1.));
#3500=DIRECTION('ref_axis',(1.,0.,0.));
#3501=DIRECTION('center_axis',(0.,0.,1.));
#3502=DIRECTION('ref_axis',(1.,0.,0.));
#3503=DIRECTION('center_axis',(0.,0.,1.));
#3504=DIRECTION('ref_axis',(1.,0.,0.));
#3505=DIRECTION('center_axis',(0.,0.,1.));
#3506=DIRECTION('ref_axis',(1.,0.,0.));
#3507=DIRECTION('',(0.,0.,-1.));
#3508=DIRECTION('center_axis',(0.,0.,1.));
#3509=DIRECTION('ref_axis',(1.,0.,0.));
#3510=DIRECTION('center_axis',(0.,0.,1.));
#3511=DIRECTION('ref_axis',(1.,0.,0.));
#3512=DIRECTION('center_axis',(0.,0.,1.));
#3513=DIRECTION('ref_axis',(1.,0.,0.));
#3514=DIRECTION('center_axis',(0.,0.,1.));
#3515=DIRECTION('ref_axis',(1.,0.,0.));
#3516=DIRECTION('',(0.,0.,-1.));
#3517=DIRECTION('center_axis',(0.,0.,1.));
#3518=DIRECTION('ref_axis',(1.,0.,0.));
#3519=DIRECTION('center_axis',(0.,0.,1.));
#3520=DIRECTION('ref_axis',(1.,0.,0.));
#3521=DIRECTION('center_axis',(0.,0.,1.));
#3522=DIRECTION('ref_axis',(1.,0.,0.));
#3523=DIRECTION('',(0.,0.,-1.));
#3524=DIRECTION('center_axis',(0.,0.,1.));
#3525=DIRECTION('ref_axis',(1.,0.,0.));
#3526=DIRECTION('axis',(0.,0.,1.));
#3527=DIRECTION('refdir',(1.,0.,0.));
#3528=DIRECTION('center_axis',(0.,0.,1.));
#3529=DIRECTION('ref_axis',(1.,0.,0.));
#3530=DIRECTION('center_axis',(0.,0.,-1.));
#3531=DIRECTION('ref_axis',(1.,0.,0.));
#3532=DIRECTION('',(0.,0.,-1.));
#3533=DIRECTION('center_axis',(0.,0.,-1.));
#3534=DIRECTION('ref_axis',(1.,0.,0.));
#3535=DIRECTION('center_axis',(0.,0.,1.));
#3536=DIRECTION('ref_axis',(1.,0.,0.));
#3537=DIRECTION('center_axis',(0.,0.,1.));
#3538=DIRECTION('ref_axis',(1.,0.,0.));
#3539=DIRECTION('',(0.,0.,-1.));
#3540=DIRECTION('center_axis',(0.,0.,1.));
#3541=DIRECTION('ref_axis',(1.,0.,0.));
#3542=DIRECTION('center_axis',(0.,0.,1.));
#3543=DIRECTION('ref_axis',(1.,0.,0.));
#3544=DIRECTION('center_axis',(0.,0.,1.));
#3545=DIRECTION('ref_axis',(1.,0.,0.));
#3546=DIRECTION('axis',(0.,0.,1.));
#3547=DIRECTION('refdir',(1.,0.,0.));
#3548=DIRECTION('center_axis',(0.,0.,1.));
#3549=DIRECTION('ref_axis',(1.,0.,0.));
#3550=DIRECTION('center_axis',(0.,0.,-1.));
#3551=DIRECTION('ref_axis',(1.,0.,0.));
#3552=DIRECTION('',(0.,0.,-1.));
#3553=DIRECTION('center_axis',(0.,0.,-1.));
#3554=DIRECTION('ref_axis',(1.,0.,0.));
#3555=DIRECTION('center_axis',(0.,0.,1.));
#3556=DIRECTION('ref_axis',(1.,0.,0.));
#3557=DIRECTION('center_axis',(0.,0.,1.));
#3558=DIRECTION('ref_axis',(1.,0.,0.));
#3559=DIRECTION('',(0.,0.,-1.));
#3560=DIRECTION('center_axis',(0.,0.,1.));
#3561=DIRECTION('ref_axis',(1.,0.,0.));
#3562=DIRECTION('center_axis',(0.,0.,1.));
#3563=DIRECTION('ref_axis',(1.,0.,0.));
#3564=DIRECTION('center_axis',(0.,0.,1.));
#3565=DIRECTION('ref_axis',(1.,0.,0.));
#3566=DIRECTION('axis',(0.,0.,1.));
#3567=DIRECTION('refdir',(1.,0.,0.));
#3568=DIRECTION('center_axis',(0.,0.,1.));
#3569=DIRECTION('ref_axis',(1.,0.,0.));
#3570=DIRECTION('center_axis',(0.,0.,-1.));
#3571=DIRECTION('ref_axis',(1.,0.,0.));
#3572=DIRECTION('',(0.,0.,-1.));
#3573=DIRECTION('center_axis',(0.,0.,-1.));
#3574=DIRECTION('ref_axis',(1.,0.,0.));
#3575=DIRECTION('center_axis',(0.,0.,1.));
#3576=DIRECTION('ref_axis',(1.,0.,0.));
#3577=DIRECTION('center_axis',(0.,0.,1.));
#3578=DIRECTION('ref_axis',(1.,0.,0.));
#3579=DIRECTION('',(0.,0.,-1.));
#3580=DIRECTION('center_axis',(0.,0.,1.));
#3581=DIRECTION('ref_axis',(1.,0.,0.));
#3582=DIRECTION('center_axis',(0.,0.,1.));
#3583=DIRECTION('ref_axis',(1.,0.,0.));
#3584=DIRECTION('center_axis',(0.,0.,1.));
#3585=DIRECTION('ref_axis',(1.,0.,0.));
#3586=DIRECTION('axis',(0.,0.,1.));
#3587=DIRECTION('refdir',(1.,0.,0.));
#3588=DIRECTION('center_axis',(-1.,0.,0.));
#3589=DIRECTION('ref_axis',(0.,1.,0.));
#3590=DIRECTION('',(0.,0.,1.));
#3591=DIRECTION('',(0.,-1.,0.));
#3592=DIRECTION('',(0.,0.,-1.));
#3593=DIRECTION('',(0.,1.,0.));
#3594=DIRECTION('center_axis',(1.,0.,0.));
#3595=DIRECTION('ref_axis',(0.,-1.,0.));
#3596=DIRECTION('',(0.,0.,-1.));
#3597=DIRECTION('',(0.,-1.,0.));
#3598=DIRECTION('',(0.,0.,1.));
#3599=DIRECTION('',(0.,1.,0.));
#3600=DIRECTION('center_axis',(0.,0.,1.));
#3601=DIRECTION('ref_axis',(1.,0.,0.));
#3602=DIRECTION('center_axis',(0.,0.,1.));
#3603=DIRECTION('ref_axis',(1.,0.,0.));
#3604=DIRECTION('center_axis',(0.,0.,-1.));
#3605=DIRECTION('ref_axis',(1.,0.,0.));
#3606=DIRECTION('center_axis',(0.,0.,1.));
#3607=DIRECTION('ref_axis',(6.12323399573677E-17,-1.,0.));
#3608=DIRECTION('center_axis',(0.,0.,-1.));
#3609=DIRECTION('ref_axis',(1.,0.,0.));
#3610=DIRECTION('center_axis',(0.,0.,1.));
#3611=DIRECTION('ref_axis',(6.12323399573677E-17,-1.,0.));
#3612=DIRECTION('center_axis',(0.,0.,1.));
#3613=DIRECTION('ref_axis',(1.,0.,0.));
#3614=DIRECTION('center_axis',(0.,0.,1.));
#3615=DIRECTION('ref_axis',(1.,0.,0.));
#3616=DIRECTION('',(0.,0.,1.));
#3617=DIRECTION('',(1.,0.,0.));
#3618=DIRECTION('',(0.,0.,1.));
#3619=DIRECTION('',(1.,0.,0.));
#3620=DIRECTION('',(0.,0.,1.));
#3621=DIRECTION('',(1.,0.,0.));
#3622=DIRECTION('',(5.61374257952022E-17,-5.39833493445635E-19,1.));
#3623=DIRECTION('',(0.948882720261885,-0.315628869383656,-5.3438220331016E-17));
#3624=DIRECTION('',(-7.62811820723666E-17,2.41750550739628E-19,1.));
#3625=DIRECTION('',(0.994320679354099,-0.106425497926025,7.58736852065524E-17));
#3626=DIRECTION('',(-1.37789476793678E-16,7.50480926595216E-20,1.));
#3627=DIRECTION('',(0.131389235726632,0.991330857350447,1.80296565579694E-17));
#3628=DIRECTION('',(2.86965558859124E-17,-9.09452108800327E-20,1.));
#3629=DIRECTION('',(0.9943206793541,-0.106425497926025,-2.85432578329549E-17));
#3630=DIRECTION('',(6.12323399582825E-17,-4.00188145704739E-33,1.));
#3631=DIRECTION('',(1.,-5.48884126349563E-33,-6.12323399582825E-17));
#3632=DIRECTION('',(6.12323399582825E-17,-4.00188145704739E-33,1.));
#3633=DIRECTION('',(1.,-5.48884126349563E-33,-6.12323399582825E-17));
#3634=DIRECTION('',(0.,0.,1.));
#3635=DIRECTION('',(1.,0.,0.));
#3636=DIRECTION('',(0.,1.,2.22044604925031E-16));
#3637=DIRECTION('',(1.,0.,0.));
#3638=DIRECTION('',(5.61374257952022E-17,-5.39833493445635E-19,1.));
#3639=DIRECTION('',(0.948882720261885,-0.315628869383656,-5.3438220331016E-17));
#3640=DIRECTION('',(0.,0.,1.));
#3641=DIRECTION('',(1.,0.,0.));
#3642=DIRECTION('',(0.,0.,1.));
#3643=DIRECTION('',(1.,0.,0.));
#3644=DIRECTION('',(0.,0.,1.));
#3645=DIRECTION('',(1.,0.,0.));
#3646=DIRECTION('',(0.,1.,2.22044604925031E-16));
#3647=DIRECTION('',(1.,0.,0.));
#3648=DIRECTION('',(-7.62811820723666E-17,2.41750550739628E-19,1.));
#3649=DIRECTION('',(0.994320679354099,-0.106425497926025,7.58736852065524E-17));
#3650=DIRECTION('',(0.,0.,1.));
#3651=DIRECTION('',(1.,0.,0.));
#3652=DIRECTION('',(0.,0.,1.));
#3653=DIRECTION('',(1.,0.,0.));
#3654=DIRECTION('',(5.61374257952022E-17,-5.39833493445635E-19,1.));
#3655=DIRECTION('',(0.948882720261885,-0.315628869383656,-5.3438220331016E-17));
#3656=DIRECTION('',(-7.62811820723666E-17,2.41750550739628E-19,1.));
#3657=DIRECTION('',(0.994320679354099,-0.106425497926025,7.58736852065524E-17));
#3658=DIRECTION('',(6.12323399582825E-17,-4.00188145704739E-33,1.));
#3659=DIRECTION('',(1.,-5.48884126349563E-33,-6.12323399582825E-17));
#3660=DIRECTION('',(0.,0.,1.));
#3661=DIRECTION('',(1.,0.,0.));
#3662=DIRECTION('',(5.61374257952022E-17,-5.39833493445635E-19,1.));
#3663=DIRECTION('',(0.948882720261885,-0.315628869383656,-5.3438220331016E-17));
#3664=DIRECTION('',(-1.37789476793678E-16,7.50480926595216E-20,1.));
#3665=DIRECTION('',(0.999979247790978,-0.00644235883751101,1.37787100846765E-16));
#3666=DIRECTION('',(-1.37789476793678E-16,7.50480926595216E-20,1.));
#3667=DIRECTION('',(0.999979247790978,-0.00644235883751101,1.37787100846765E-16));
#3668=DIRECTION('',(-7.62811820723666E-17,2.41750550739628E-19,1.));
#3669=DIRECTION('',(0.994320679354099,-0.106425497926025,7.58736852065524E-17));
#3670=DIRECTION('',(0.,0.,1.));
#3671=DIRECTION('',(1.,0.,0.));
#3672=DIRECTION('',(0.,0.,1.));
#3673=DIRECTION('',(1.,0.,0.));
#3674=DIRECTION('',(5.61374257952022E-17,-5.39833493445635E-19,1.));
#3675=DIRECTION('',(0.948882720261885,-0.315628869383656,-5.3438220331016E-17));
#3676=DIRECTION('',(5.61374257952022E-17,-5.39833493445635E-19,1.));
#3677=DIRECTION('',(0.948882720261885,-0.315628869383656,-5.3438220331016E-17));
#3678=DIRECTION('',(-7.62811820723666E-17,2.41750550739628E-19,1.));
#3679=DIRECTION('',(0.994320679354099,-0.106425497926025,7.58736852065524E-17));
#3680=DIRECTION('',(-7.62811820723666E-17,2.41750550739628E-19,1.));
#3681=DIRECTION('',(0.994320679354099,-0.106425497926025,7.58736852065524E-17));
#3682=DIRECTION('',(6.12323399582825E-17,-4.00188145704739E-33,1.));
#3683=DIRECTION('',(1.,-5.48884126349563E-33,-6.12323399582825E-17));
#3684=DIRECTION('',(0.,1.,2.22044604925031E-16));
#3685=DIRECTION('',(1.,0.,0.));
#3686=DIRECTION('',(0.,1.,2.22044604925031E-16));
#3687=DIRECTION('',(1.,0.,0.));
#3688=DIRECTION('',(0.,0.,1.));
#3689=DIRECTION('',(1.,0.,0.));
#3690=DIRECTION('',(5.61374257952022E-17,-5.39833493445635E-19,1.));
#3691=DIRECTION('',(0.948882720261885,-0.315628869383656,-5.3438220331016E-17));
#3692=DIRECTION('',(-7.62811820723666E-17,2.41750550739628E-19,1.));
#3693=DIRECTION('',(0.994320679354099,-0.106425497926025,7.58736852065524E-17));
#3694=DIRECTION('',(6.12323399582825E-17,-4.00188145704739E-33,1.));
#3695=DIRECTION('',(1.,-5.48884126349563E-33,-6.12323399582825E-17));
#3696=DIRECTION('',(0.,1.,2.22044604925031E-16));
#3697=DIRECTION('',(1.,0.,0.));
#3698=DIRECTION('',(0.,1.,2.22044604925031E-16));
#3699=DIRECTION('',(1.,0.,0.));
#3700=CARTESIAN_POINT('',(0.,0.,0.));
#3701=CARTESIAN_POINT('',(0.,0.,0.));
#3702=CARTESIAN_POINT('Origin',(0.,0.,5.));
#3703=CARTESIAN_POINT('',(-5.,6.12323399573677E-16,10.));
#3704=CARTESIAN_POINT('Origin',(0.,0.,10.));
#3705=CARTESIAN_POINT('',(-5.,6.12323399573677E-16,0.));
#3706=CARTESIAN_POINT('',(-5.,6.12323399573677E-16,5.));
#3707=CARTESIAN_POINT('Origin',(0.,0.,0.));
#3708=CARTESIAN_POINT('Origin',(80.,0.,5.));
#3709=CARTESIAN_POINT('',(75.,6.12323399573677E-16,10.));
#3710=CARTESIAN_POINT('Origin',(80.,0.,10.));
#3711=CARTESIAN_POINT('',(75.,6.12323399573677E-16,0.));
#3712=CARTESIAN_POINT('',(75.,6.12323399573677E-16,5.));
#3713=CARTESIAN_POINT('Origin',(80.,0.,0.));
#3714=CARTESIAN_POINT('Origin',(240.,315.,0.));
#3715=CARTESIAN_POINT('',(245.,315.,0.));
#3716=CARTESIAN_POINT('',(-76.,315.,0.));
#3717=CARTESIAN_POINT('',(160.,315.,0.));
#3718=CARTESIAN_POINT('',(-76.,315.,10.));
#3719=CARTESIAN_POINT('',(-76.,315.,0.));
#3720=CARTESIAN_POINT('',(245.,315.,10.));
#3721=CARTESIAN_POINT('',(160.,315.,10.));
#3722=CARTESIAN_POINT('',(245.,315.,0.));
#3723=CARTESIAN_POINT('Origin',(245.,-150.,0.));
#3724=CARTESIAN_POINT('',(245.,-155.,0.));
#3725=CARTESIAN_POINT('',(245.,-35.,0.));
#3726=CARTESIAN_POINT('',(245.,-155.,10.));
#3727=CARTESIAN_POINT('',(245.,-35.,10.));
#3728=CARTESIAN_POINT('',(245.,-155.,0.));
#3729=CARTESIAN_POINT('Origin',(-80.,-155.,0.));
#3730=CARTESIAN_POINT('',(-76.,-155.,0.));
#3731=CARTESIAN_POINT('',(0.,-155.,0.));
#3732=CARTESIAN_POINT('',(-76.,-155.,10.));
#3733=CARTESIAN_POINT('',(0.,-155.,10.));
#3734=CARTESIAN_POINT('',(-76.,-155.,0.));
#3735=CARTESIAN_POINT('Origin',(-76.,310.,0.));
#3736=CARTESIAN_POINT('',(-76.,195.,0.));
#3737=CARTESIAN_POINT('',(-76.,195.,10.));
#3738=CARTESIAN_POINT('Origin',(80.,80.,10.));
#3739=CARTESIAN_POINT('Origin',(80.,80.,0.));
#3740=CARTESIAN_POINT('',(0.,0.,0.));
#3741=CARTESIAN_POINT('Origin',(0.,0.,0.));
#3742=CARTESIAN_POINT('',(-5.,-6.12323399573677E-16,10.));
#3743=CARTESIAN_POINT('Origin',(0.,0.,10.));
#3744=CARTESIAN_POINT('',(-5.,-6.12323399573677E-16,0.));
#3745=CARTESIAN_POINT('',(-5.,-6.12323399573677E-16,0.));
#3746=CARTESIAN_POINT('Origin',(0.,0.,0.));
#3747=CARTESIAN_POINT('Origin',(0.,0.,0.));
#3748=CARTESIAN_POINT('',(-12.,-1.46957615897682E-15,10.));
#3749=CARTESIAN_POINT('Origin',(0.,0.,10.));
#3750=CARTESIAN_POINT('',(-12.,-1.46957615897682E-15,0.));
#3751=CARTESIAN_POINT('',(-12.,-1.46957615897682E-15,0.));
#3752=CARTESIAN_POINT('Origin',(0.,0.,0.));
#3753=CARTESIAN_POINT('Origin',(0.,0.,10.));
#3754=CARTESIAN_POINT('Origin',(0.,0.,0.));
#3755=CARTESIAN_POINT('',(0.,0.,0.));
#3756=CARTESIAN_POINT('Origin',(0.,0.,0.));
#3757=CARTESIAN_POINT('',(-5.,-6.12323399573677E-16,26.));
#3758=CARTESIAN_POINT('Origin',(0.,0.,26.));
#3759=CARTESIAN_POINT('',(-5.,-6.12323399573677E-16,0.));
#3760=CARTESIAN_POINT('',(-5.,-6.12323399573677E-16,0.));
#3761=CARTESIAN_POINT('Origin',(0.,0.,0.));
#3762=CARTESIAN_POINT('Origin',(0.,0.,0.));
#3763=CARTESIAN_POINT('',(-12.,-1.46957615897682E-15,26.));
#3764=CARTESIAN_POINT('Origin',(0.,0.,26.));
#3765=CARTESIAN_POINT('',(-12.,-1.46957615897682E-15,0.));
#3766=CARTESIAN_POINT('',(-12.,-1.46957615897682E-15,0.));
#3767=CARTESIAN_POINT('Origin',(0.,0.,0.));
#3768=CARTESIAN_POINT('Origin',(0.,0.,26.));
#3769=CARTESIAN_POINT('Origin',(0.,0.,0.));
#3770=CARTESIAN_POINT('',(0.,0.,0.));
#3771=CARTESIAN_POINT('Origin',(0.,0.,4.));
#3772=CARTESIAN_POINT('',(-7.,8.57252759403147E-16,8.));
#3773=CARTESIAN_POINT('Origin',(0.,0.,8.));
#3774=CARTESIAN_POINT('',(-7.,8.57252759403147E-16,0.));
#3775=CARTESIAN_POINT('',(-7.,8.57252759403147E-16,4.));
#3776=CARTESIAN_POINT('Origin',(0.,0.,0.));
#3777=CARTESIAN_POINT('Origin',(40.,0.,4.));
#3778=CARTESIAN_POINT('',(33.,8.57252759403147E-16,8.));
#3779=CARTESIAN_POINT('Origin',(40.,0.,8.));
#3780=CARTESIAN_POINT('',(33.,8.57252759403147E-16,0.));
#3781=CARTESIAN_POINT('',(33.,8.57252759403147E-16,4.));
#3782=CARTESIAN_POINT('Origin',(40.,0.,0.));
#3783=CARTESIAN_POINT('Origin',(40.,12.,0.));
#3784=CARTESIAN_POINT('',(40.,12.,0.));
#3785=CARTESIAN_POINT('',(0.,12.,0.));
#3786=CARTESIAN_POINT('',(40.,12.,0.));
#3787=CARTESIAN_POINT('',(0.,12.,8.));
#3788=CARTESIAN_POINT('',(0.,12.,0.));
#3789=CARTESIAN_POINT('',(40.,12.,8.));
#3790=CARTESIAN_POINT('',(40.,12.,8.));
#3791=CARTESIAN_POINT('',(40.,12.,0.));
#3792=CARTESIAN_POINT('Origin',(40.,0.,0.));
#3793=CARTESIAN_POINT('',(40.,-12.,0.));
#3794=CARTESIAN_POINT('Origin',(40.,0.,0.));
#3795=CARTESIAN_POINT('',(40.,-12.,8.));
#3796=CARTESIAN_POINT('Origin',(40.,0.,8.));
#3797=CARTESIAN_POINT('',(40.,-12.,0.));
#3798=CARTESIAN_POINT('Origin',(0.,-12.,0.));
#3799=CARTESIAN_POINT('',(-1.46957615897682E-15,-12.,0.));
#3800=CARTESIAN_POINT('',(0.,-12.,0.));
#3801=CARTESIAN_POINT('',(-1.46957615897682E-15,-12.,8.));
#3802=CARTESIAN_POINT('',(0.,-12.,8.));
#3803=CARTESIAN_POINT('',(-1.46957615897682E-15,-12.,0.));
#3804=CARTESIAN_POINT('Origin',(0.,0.,0.));
#3805=CARTESIAN_POINT('Origin',(0.,0.,0.));
#3806=CARTESIAN_POINT('Origin',(0.,0.,8.));
#3807=CARTESIAN_POINT('Origin',(20.,0.,8.));
#3808=CARTESIAN_POINT('Origin',(20.,0.,0.));
#3809=CARTESIAN_POINT('',(0.,0.,0.));
#3810=CARTESIAN_POINT('Origin',(150.,-7.,10.));
#3811=CARTESIAN_POINT('',(150.,-7.,10.));
#3812=CARTESIAN_POINT('',(30.,-7.,10.));
#3813=CARTESIAN_POINT('',(120.,-7.,10.));
#3814=CARTESIAN_POINT('',(150.,-7.,0.));
#3815=CARTESIAN_POINT('',(150.,-7.,10.));
#3816=CARTESIAN_POINT('',(30.,-7.,0.));
#3817=CARTESIAN_POINT('',(120.,-7.,0.));
#3818=CARTESIAN_POINT('',(30.,-7.,10.));
#3819=CARTESIAN_POINT('Origin',(150.,0.,10.));
#3820=CARTESIAN_POINT('',(150.,7.,10.));
#3821=CARTESIAN_POINT('Origin',(150.,0.,10.));
#3822=CARTESIAN_POINT('',(150.,7.,0.));
#3823=CARTESIAN_POINT('',(150.,7.,10.));
#3824=CARTESIAN_POINT('Origin',(150.,0.,0.));
#3825=CARTESIAN_POINT('Origin',(30.,7.,10.));
#3826=CARTESIAN_POINT('',(30.,7.,10.));
#3827=CARTESIAN_POINT('',(60.,7.,10.));
#3828=CARTESIAN_POINT('',(30.,7.,0.));
#3829=CARTESIAN_POINT('',(30.,7.,10.));
#3830=CARTESIAN_POINT('',(60.,7.,0.));
#3831=CARTESIAN_POINT('Origin',(30.,0.,10.));
#3832=CARTESIAN_POINT('Origin',(30.,0.,10.));
#3833=CARTESIAN_POINT('Origin',(30.,0.,0.));
#3834=CARTESIAN_POINT('Origin',(0.,0.,5.));
#3835=CARTESIAN_POINT('',(-7.,8.57252759403147E-16,10.));
#3836=CARTESIAN_POINT('Origin',(0.,0.,10.));
#3837=CARTESIAN_POINT('',(-7.,8.57252759403147E-16,0.));
#3838=CARTESIAN_POINT('',(-7.,8.57252759403147E-16,5.));
#3839=CARTESIAN_POINT('Origin',(0.,0.,0.));
#3840=CARTESIAN_POINT('Origin',(180.,0.,5.));
#3841=CARTESIAN_POINT('',(173.,8.57252759403147E-16,10.));
#3842=CARTESIAN_POINT('Origin',(180.,0.,10.));
#3843=CARTESIAN_POINT('',(173.,8.57252759403147E-16,0.));
#3844=CARTESIAN_POINT('',(173.,8.57252759403147E-16,5.));
#3845=CARTESIAN_POINT('Origin',(180.,0.,0.));
#3846=CARTESIAN_POINT('Origin',(180.,15.,0.));
#3847=CARTESIAN_POINT('',(180.,15.,0.));
#3848=CARTESIAN_POINT('',(0.,15.,0.));
#3849=CARTESIAN_POINT('',(180.,15.,0.));
#3850=CARTESIAN_POINT('',(0.,15.,10.));
#3851=CARTESIAN_POINT('',(0.,15.,0.));
#3852=CARTESIAN_POINT('',(180.,15.,10.));
#3853=CARTESIAN_POINT('',(180.,15.,10.));
#3854=CARTESIAN_POINT('',(180.,15.,0.));
#3855=CARTESIAN_POINT('Origin',(180.,0.,0.));
#3856=CARTESIAN_POINT('',(180.,-15.,0.));
#3857=CARTESIAN_POINT('Origin',(180.,0.,0.));
#3858=CARTESIAN_POINT('',(180.,-15.,10.));
#3859=CARTESIAN_POINT('Origin',(180.,0.,10.));
#3860=CARTESIAN_POINT('',(180.,-15.,0.));
#3861=CARTESIAN_POINT('Origin',(0.,-15.,0.));
#3862=CARTESIAN_POINT('',(-1.83697019872103E-15,-15.,0.));
#3863=CARTESIAN_POINT('',(0.,-15.,0.));
#3864=CARTESIAN_POINT('',(-1.83697019872103E-15,-15.,10.));
#3865=CARTESIAN_POINT('',(0.,-15.,10.));
#3866=CARTESIAN_POINT('',(-1.83697019872103E-15,-15.,0.));
#3867=CARTESIAN_POINT('Origin',(0.,0.,0.));
#3868=CARTESIAN_POINT('Origin',(0.,0.,0.));
#3869=CARTESIAN_POINT('Origin',(0.,0.,10.));
#3870=CARTESIAN_POINT('Origin',(90.,0.,10.));
#3871=CARTESIAN_POINT('Origin',(90.,0.,0.));
#3872=CARTESIAN_POINT('',(0.,0.,0.));
#3873=CARTESIAN_POINT('Origin',(0.,0.,4.));
#3874=CARTESIAN_POINT('',(-7.,8.57252759403147E-16,8.));
#3875=CARTESIAN_POINT('Origin',(0.,0.,8.));
#3876=CARTESIAN_POINT('',(-7.,8.57252759403147E-16,0.));
#3877=CARTESIAN_POINT('',(-7.,8.57252759403147E-16,4.));
#3878=CARTESIAN_POINT('Origin',(0.,0.,0.));
#3879=CARTESIAN_POINT('Origin',(160.,0.,4.));
#3880=CARTESIAN_POINT('',(153.,8.57252759403147E-16,8.));
#3881=CARTESIAN_POINT('Origin',(160.,0.,8.));
#3882=CARTESIAN_POINT('',(153.,8.57252759403147E-16,0.));
#3883=CARTESIAN_POINT('',(153.,8.57252759403147E-16,4.));
#3884=CARTESIAN_POINT('Origin',(160.,0.,0.));
#3885=CARTESIAN_POINT('Origin',(160.,12.,0.));
#3886=CARTESIAN_POINT('',(160.,12.,0.));
#3887=CARTESIAN_POINT('',(0.,12.,0.));
#3888=CARTESIAN_POINT('',(160.,12.,0.));
#3889=CARTESIAN_POINT('',(0.,12.,8.));
#3890=CARTESIAN_POINT('',(0.,12.,0.));
#3891=CARTESIAN_POINT('',(160.,12.,8.));
#3892=CARTESIAN_POINT('',(160.,12.,8.));
#3893=CARTESIAN_POINT('',(160.,12.,0.));
#3894=CARTESIAN_POINT('Origin',(160.,-1.11022302462516E-15,0.));
#3895=CARTESIAN_POINT('',(160.,-12.,0.));
#3896=CARTESIAN_POINT('Origin',(160.,-1.11022302462516E-15,0.));
#3897=CARTESIAN_POINT('',(160.,-12.,8.));
#3898=CARTESIAN_POINT('Origin',(160.,-1.11022302462516E-15,8.));
#3899=CARTESIAN_POINT('',(160.,-12.,0.));
#3900=CARTESIAN_POINT('Origin',(0.,-12.,0.));
#3901=CARTESIAN_POINT('',(-1.46957615897682E-15,-12.,0.));
#3902=CARTESIAN_POINT('',(0.,-12.,0.));
#3903=CARTESIAN_POINT('',(-1.46957615897682E-15,-12.,8.));
#3904=CARTESIAN_POINT('',(0.,-12.,8.));
#3905=CARTESIAN_POINT('',(-1.46957615897682E-15,-12.,0.));
#3906=CARTESIAN_POINT('Origin',(0.,0.,0.));
#3907=CARTESIAN_POINT('Origin',(0.,0.,0.));
#3908=CARTESIAN_POINT('Origin',(0.,0.,8.));
#3909=CARTESIAN_POINT('Origin',(80.,0.,8.));
#3910=CARTESIAN_POINT('Origin',(80.,0.,0.));
#3911=CARTESIAN_POINT('',(0.,0.,0.));
#3912=CARTESIAN_POINT('Origin',(0.,0.,5.));
#3913=CARTESIAN_POINT('',(-5.,6.12323399573677E-16,10.));
#3914=CARTESIAN_POINT('Origin',(0.,0.,10.));
#3915=CARTESIAN_POINT('',(-5.,6.12323399573677E-16,0.));
#3916=CARTESIAN_POINT('',(-5.,6.12323399573677E-16,5.));
#3917=CARTESIAN_POINT('Origin',(0.,0.,0.));
#3918=CARTESIAN_POINT('Origin',(8.,6.,0.));
#3919=CARTESIAN_POINT('',(8.,6.,0.));
#3920=CARTESIAN_POINT('',(-8.,6.,0.));
#3921=CARTESIAN_POINT('',(8.,6.,0.));
#3922=CARTESIAN_POINT('',(-8.,6.,10.));
#3923=CARTESIAN_POINT('',(-8.,6.,0.));
#3924=CARTESIAN_POINT('',(8.,6.,10.));
#3925=CARTESIAN_POINT('',(8.,6.,10.));
#3926=CARTESIAN_POINT('',(8.,6.,0.));
#3927=CARTESIAN_POINT('Origin',(8.,-6.,0.));
#3928=CARTESIAN_POINT('',(8.,-6.,0.));
#3929=CARTESIAN_POINT('',(8.,-6.,0.));
#3930=CARTESIAN_POINT('',(8.,-6.,10.));
#3931=CARTESIAN_POINT('',(8.,-6.,10.));
#3932=CARTESIAN_POINT('',(8.,-6.,0.));
#3933=CARTESIAN_POINT('Origin',(-8.,-6.,0.));
#3934=CARTESIAN_POINT('',(-8.,-6.,0.));
#3935=CARTESIAN_POINT('',(-8.,-6.,0.));
#3936=CARTESIAN_POINT('',(-8.,-6.,10.));
#3937=CARTESIAN_POINT('',(-8.,-6.,10.));
#3938=CARTESIAN_POINT('',(-8.,-6.,0.));
#3939=CARTESIAN_POINT('Origin',(-8.,6.,0.));
#3940=CARTESIAN_POINT('',(-8.,6.,0.));
#3941=CARTESIAN_POINT('',(-8.,6.,10.));
#3942=CARTESIAN_POINT('Origin',(0.,0.,10.));
#3943=CARTESIAN_POINT('Origin',(0.,0.,0.));
#3944=CARTESIAN_POINT('',(0.,0.,0.));
#3945=CARTESIAN_POINT('Origin',(0.,0.,8.));
#3946=CARTESIAN_POINT('',(-5.,6.12323399573677E-16,16.));
#3947=CARTESIAN_POINT('Origin',(0.,0.,16.));
#3948=CARTESIAN_POINT('',(-5.,6.12323399573677E-16,0.));
#3949=CARTESIAN_POINT('',(-5.,6.12323399573677E-16,8.));
#3950=CARTESIAN_POINT('Origin',(0.,0.,0.));
#3951=CARTESIAN_POINT('Origin',(-20.,0.,8.));
#3952=CARTESIAN_POINT('',(-20.,20.,3.));
#3953=CARTESIAN_POINT('Origin',(-20.,20.,8.));
#3954=CARTESIAN_POINT('',(-20.,-20.,3.));
#3955=CARTESIAN_POINT('',(-20.,0.,3.));
#3956=CARTESIAN_POINT('Origin',(-20.,-20.,8.));
#3957=CARTESIAN_POINT('Origin',(20.,0.,8.));
#3958=CARTESIAN_POINT('',(20.,20.,3.));
#3959=CARTESIAN_POINT('Origin',(20.,20.,8.));
#3960=CARTESIAN_POINT('',(20.,-20.,3.));
#3961=CARTESIAN_POINT('',(20.,0.,3.));
#3962=CARTESIAN_POINT('Origin',(20.,-20.,8.));
#3963=CARTESIAN_POINT('Origin',(30.,20.,0.));
#3964=CARTESIAN_POINT('',(30.,20.,0.));
#3965=CARTESIAN_POINT('',(-30.,20.,0.));
#3966=CARTESIAN_POINT('',(30.,20.,0.));
#3967=CARTESIAN_POINT('',(-30.,20.,16.));
#3968=CARTESIAN_POINT('',(-30.,20.,0.));
#3969=CARTESIAN_POINT('',(30.,20.,16.));
#3970=CARTESIAN_POINT('',(30.,20.,16.));
#3971=CARTESIAN_POINT('',(30.,20.,0.));
#3972=CARTESIAN_POINT('Origin',(30.,-20.,0.));
#3973=CARTESIAN_POINT('',(30.,-20.,0.));
#3974=CARTESIAN_POINT('',(30.,-20.,0.));
#3975=CARTESIAN_POINT('',(30.,-20.,16.));
#3976=CARTESIAN_POINT('',(30.,-20.,16.));
#3977=CARTESIAN_POINT('',(30.,-20.,0.));
#3978=CARTESIAN_POINT('Origin',(-30.,-20.,0.));
#3979=CARTESIAN_POINT('',(-30.,-20.,0.));
#3980=CARTESIAN_POINT('',(-30.,-20.,0.));
#3981=CARTESIAN_POINT('',(-30.,-20.,16.));
#3982=CARTESIAN_POINT('',(-30.,-20.,16.));
#3983=CARTESIAN_POINT('',(-30.,-20.,0.));
#3984=CARTESIAN_POINT('Origin',(-30.,20.,0.));
#3985=CARTESIAN_POINT('',(-30.,20.,0.));
#3986=CARTESIAN_POINT('',(-30.,20.,16.));
#3987=CARTESIAN_POINT('Origin',(0.,0.,16.));
#3988=CARTESIAN_POINT('Origin',(0.,0.,0.));
#3989=CARTESIAN_POINT('',(0.,0.,0.));
#3990=CARTESIAN_POINT('Origin',(0.,0.,0.));
#3991=CARTESIAN_POINT('',(-5.,-6.12323399573677E-16,14.));
#3992=CARTESIAN_POINT('Origin',(0.,0.,14.));
#3993=CARTESIAN_POINT('',(-5.,-6.12323399573677E-16,0.));
#3994=CARTESIAN_POINT('',(-5.,-6.12323399573677E-16,0.));
#3995=CARTESIAN_POINT('Origin',(0.,0.,0.));
#3996=CARTESIAN_POINT('Origin',(0.,0.,0.));
#3997=CARTESIAN_POINT('',(-12.,-1.46957615897682E-15,14.));
#3998=CARTESIAN_POINT('Origin',(0.,0.,14.));
#3999=CARTESIAN_POINT('',(-12.,-1.46957615897682E-15,0.));
#4000=CARTESIAN_POINT('',(-12.,-1.46957615897682E-15,0.));
#4001=CARTESIAN_POINT('Origin',(0.,0.,0.));
#4002=CARTESIAN_POINT('Origin',(0.,0.,14.));
#4003=CARTESIAN_POINT('Origin',(0.,0.,0.));
#4004=CARTESIAN_POINT('',(0.,0.,0.));
#4005=CARTESIAN_POINT('Origin',(0.,0.,14.));
#4006=CARTESIAN_POINT('',(6.12323399573677E-16,10.,9.));
#4007=CARTESIAN_POINT('Origin',(0.,10.,14.));
#4008=CARTESIAN_POINT('',(6.12323399573677E-16,-10.,9.));
#4009=CARTESIAN_POINT('',(6.12323399573677E-16,0.,9.));
#4010=CARTESIAN_POINT('Origin',(0.,-10.,14.));
#4011=CARTESIAN_POINT('Origin',(10.,10.,0.));
#4012=CARTESIAN_POINT('',(10.,10.,0.));
#4013=CARTESIAN_POINT('',(-10.,10.,0.));
#4014=CARTESIAN_POINT('',(10.,10.,0.));
#4015=CARTESIAN_POINT('',(-10.,10.,30.));
#4016=CARTESIAN_POINT('',(-10.,10.,0.));
#4017=CARTESIAN_POINT('',(10.,10.,30.));
#4018=CARTESIAN_POINT('',(10.,10.,30.));
#4019=CARTESIAN_POINT('',(10.,10.,0.));
#4020=CARTESIAN_POINT('Origin',(10.,-10.,0.));
#4021=CARTESIAN_POINT('',(10.,-10.,0.));
#4022=CARTESIAN_POINT('',(10.,-10.,0.));
#4023=CARTESIAN_POINT('',(10.,-10.,30.));
#4024=CARTESIAN_POINT('',(10.,-10.,30.));
#4025=CARTESIAN_POINT('',(10.,-10.,0.));
#4026=CARTESIAN_POINT('Origin',(-10.,-10.,0.));
#4027=CARTESIAN_POINT('',(-10.,-10.,0.));
#4028=CARTESIAN_POINT('',(-10.,-10.,0.));
#4029=CARTESIAN_POINT('',(-10.,-10.,30.));
#4030=CARTESIAN_POINT('',(-10.,-10.,30.));
#4031=CARTESIAN_POINT('',(-10.,-10.,0.));
#4032=CARTESIAN_POINT('Origin',(-10.,10.,0.));
#4033=CARTESIAN_POINT('',(-10.,10.,0.));
#4034=CARTESIAN_POINT('',(-10.,10.,30.));
#4035=CARTESIAN_POINT('Origin',(0.,0.,30.));
#4036=CARTESIAN_POINT('Origin',(0.,0.,0.));
#4037=CARTESIAN_POINT('',(0.,0.,0.));
#4038=CARTESIAN_POINT('Origin',(0.,0.,433.));
#4039=CARTESIAN_POINT('',(-4.,-4.89858719658941E-16,432.));
#4040=CARTESIAN_POINT('Origin',(0.,0.,432.));
#4041=CARTESIAN_POINT('',(-4.,-4.89858719658941E-16,434.));
#4042=CARTESIAN_POINT('',(-4.,-4.89858719658941E-16,433.));
#4043=CARTESIAN_POINT('Origin',(0.,0.,434.));
#4044=CARTESIAN_POINT('Origin',(8.,0.,432.));
#4045=CARTESIAN_POINT('',(-5.,6.12323399573677E-16,432.));
#4046=CARTESIAN_POINT('Origin',(0.,0.,432.));
#4047=CARTESIAN_POINT('Origin',(4.,0.,434.));
#4048=CARTESIAN_POINT('',(-5.,-6.12323399573677E-16,434.));
#4049=CARTESIAN_POINT('Origin',(0.,0.,434.));
#4050=CARTESIAN_POINT('Origin',(0.,0.,0.));
#4051=CARTESIAN_POINT('',(-5.,-6.12323399573677E-16,435.));
#4052=CARTESIAN_POINT('Origin',(0.,0.,435.));
#4053=CARTESIAN_POINT('',(-5.,-6.12323399573677E-16,0.));
#4054=CARTESIAN_POINT('Origin',(0.,0.,0.));
#4055=CARTESIAN_POINT('',(-8.,-9.79717439317883E-16,0.));
#4056=CARTESIAN_POINT('Origin',(0.,0.,0.));
#4057=CARTESIAN_POINT('',(-5.,-6.12323399573677E-16,0.));
#4058=CARTESIAN_POINT('Origin',(0.,0.,0.));
#4059=CARTESIAN_POINT('Origin',(0.,0.,-2.));
#4060=CARTESIAN_POINT('',(-8.,-9.79717439317883E-16,-7.));
#4061=CARTESIAN_POINT('',(-8.,-9.79717439317883E-16,-2.));
#4062=CARTESIAN_POINT('Origin',(0.,0.,-7.));
#4063=CARTESIAN_POINT('Origin',(0.,0.,-7.));
#4064=CARTESIAN_POINT('Origin',(0.,0.,0.));
#4065=CARTESIAN_POINT('',(-5.,-6.12323399573677E-16,0.));
#4066=CARTESIAN_POINT('Origin',(0.,0.,435.));
#4067=CARTESIAN_POINT('',(0.,0.,0.));
#4068=CARTESIAN_POINT('Origin',(0.,0.,31.));
#4069=CARTESIAN_POINT('',(-4.,-4.89858719658941E-16,30.));
#4070=CARTESIAN_POINT('Origin',(0.,0.,30.));
#4071=CARTESIAN_POINT('',(-4.,-4.89858719658941E-16,32.));
#4072=CARTESIAN_POINT('',(-4.,-4.89858719658941E-16,31.));
#4073=CARTESIAN_POINT('Origin',(0.,0.,32.));
#4074=CARTESIAN_POINT('Origin',(8.,0.,30.));
#4075=CARTESIAN_POINT('',(-5.,6.12323399573677E-16,30.));
#4076=CARTESIAN_POINT('Origin',(0.,0.,30.));
#4077=CARTESIAN_POINT('Origin',(4.,0.,32.));
#4078=CARTESIAN_POINT('',(-5.,-6.12323399573677E-16,32.));
#4079=CARTESIAN_POINT('Origin',(0.,0.,32.));
#4080=CARTESIAN_POINT('Origin',(0.,0.,0.));
#4081=CARTESIAN_POINT('',(-5.,-6.12323399573677E-16,33.));
#4082=CARTESIAN_POINT('Origin',(0.,0.,33.));
#4083=CARTESIAN_POINT('',(-5.,-6.12323399573677E-16,0.));
#4084=CARTESIAN_POINT('Origin',(0.,0.,0.));
#4085=CARTESIAN_POINT('',(-8.,-9.79717439317883E-16,0.));
#4086=CARTESIAN_POINT('Origin',(0.,0.,0.));
#4087=CARTESIAN_POINT('',(-5.,-6.12323399573677E-16,0.));
#4088=CARTESIAN_POINT('Origin',(0.,0.,0.));
#4089=CARTESIAN_POINT('Origin',(0.,0.,-4.));
#4090=CARTESIAN_POINT('',(-8.,-9.79717439317883E-16,-4.));
#4091=CARTESIAN_POINT('',(-8.,-9.79717439317883E-16,-4.));
#4092=CARTESIAN_POINT('Origin',(0.,0.,-4.));
#4093=CARTESIAN_POINT('Origin',(0.,0.,-4.));
#4094=CARTESIAN_POINT('Origin',(0.,0.,0.));
#4095=CARTESIAN_POINT('',(-5.,-6.12323399573677E-16,0.));
#4096=CARTESIAN_POINT('Origin',(0.,0.,33.));
#4097=CARTESIAN_POINT('',(0.,0.,0.));
#4098=CARTESIAN_POINT('Origin',(0.,0.,49.));
#4099=CARTESIAN_POINT('',(-4.,-4.89858719658941E-16,48.));
#4100=CARTESIAN_POINT('Origin',(0.,0.,48.));
#4101=CARTESIAN_POINT('',(-4.,-4.89858719658941E-16,50.));
#4102=CARTESIAN_POINT('',(-4.,-4.89858719658941E-16,49.));
#4103=CARTESIAN_POINT('Origin',(0.,0.,50.));
#4104=CARTESIAN_POINT('Origin',(8.,0.,48.));
#4105=CARTESIAN_POINT('',(-5.,6.12323399573677E-16,48.));
#4106=CARTESIAN_POINT('Origin',(0.,0.,48.));
#4107=CARTESIAN_POINT('Origin',(4.,0.,50.));
#4108=CARTESIAN_POINT('',(-5.,-6.12323399573677E-16,50.));
#4109=CARTESIAN_POINT('Origin',(0.,0.,50.));
#4110=CARTESIAN_POINT('Origin',(0.,0.,0.));
#4111=CARTESIAN_POINT('',(-5.,-6.12323399573677E-16,51.));
#4112=CARTESIAN_POINT('Origin',(0.,0.,51.));
#4113=CARTESIAN_POINT('',(-5.,-6.12323399573677E-16,0.));
#4114=CARTESIAN_POINT('Origin',(0.,0.,0.));
#4115=CARTESIAN_POINT('',(-8.,-9.79717439317883E-16,0.));
#4116=CARTESIAN_POINT('Origin',(0.,0.,0.));
#4117=CARTESIAN_POINT('',(-5.,-6.12323399573677E-16,0.));
#4118=CARTESIAN_POINT('Origin',(0.,0.,0.));
#4119=CARTESIAN_POINT('Origin',(0.,0.,-4.));
#4120=CARTESIAN_POINT('',(-8.,-9.79717439317883E-16,-4.));
#4121=CARTESIAN_POINT('',(-8.,-9.79717439317883E-16,-4.));
#4122=CARTESIAN_POINT('Origin',(0.,0.,-4.));
#4123=CARTESIAN_POINT('Origin',(0.,0.,-4.));
#4124=CARTESIAN_POINT('Origin',(0.,0.,0.));
#4125=CARTESIAN_POINT('',(-5.,-6.12323399573677E-16,0.));
#4126=CARTESIAN_POINT('Origin',(0.,0.,51.));
#4127=CARTESIAN_POINT('',(0.,0.,0.));
#4128=CARTESIAN_POINT('Origin',(0.,0.,18.));
#4129=CARTESIAN_POINT('',(-7.,-8.57252759403147E-16,18.));
#4130=CARTESIAN_POINT('Origin',(0.,0.,18.));
#4131=CARTESIAN_POINT('',(-5.,-6.12323399573677E-16,18.));
#4132=CARTESIAN_POINT('Origin',(0.,0.,18.));
#4133=CARTESIAN_POINT('Origin',(0.,0.,10.));
#4134=CARTESIAN_POINT('',(-7.,-8.57252759403147E-16,10.));
#4135=CARTESIAN_POINT('Origin',(0.,0.,10.));
#4136=CARTESIAN_POINT('',(-5.,6.12323399573677E-16,10.));
#4137=CARTESIAN_POINT('Origin',(0.,0.,10.));
#4138=CARTESIAN_POINT('Origin',(0.,0.,10.));
#4139=CARTESIAN_POINT('',(-7.,-8.57252759403147E-16,10.));
#4140=CARTESIAN_POINT('Origin',(0.,0.,0.));
#4141=CARTESIAN_POINT('',(-5.,-6.12323399573677E-16,0.));
#4142=CARTESIAN_POINT('',(-5.,-6.12323399573677E-16,0.));
#4143=CARTESIAN_POINT('Origin',(0.,0.,0.));
#4144=CARTESIAN_POINT('Origin',(0.,0.,31.));
#4145=CARTESIAN_POINT('',(-4.,-4.89858719658941E-16,30.));
#4146=CARTESIAN_POINT('Origin',(0.,0.,30.));
#4147=CARTESIAN_POINT('',(-4.,-4.89858719658941E-16,32.));
#4148=CARTESIAN_POINT('',(-4.,-4.89858719658941E-16,31.));
#4149=CARTESIAN_POINT('Origin',(0.,0.,32.));
#4150=CARTESIAN_POINT('Origin',(8.,0.,30.));
#4151=CARTESIAN_POINT('',(-5.,6.12323399573677E-16,30.));
#4152=CARTESIAN_POINT('Origin',(0.,0.,30.));
#4153=CARTESIAN_POINT('Origin',(4.,0.,32.));
#4154=CARTESIAN_POINT('',(-5.,-6.12323399573677E-16,32.));
#4155=CARTESIAN_POINT('Origin',(0.,0.,32.));
#4156=CARTESIAN_POINT('Origin',(0.,0.,0.));
#4157=CARTESIAN_POINT('',(-5.,-6.12323399573677E-16,33.));
#4158=CARTESIAN_POINT('Origin',(0.,0.,33.));
#4159=CARTESIAN_POINT('',(-5.,-6.12323399573677E-16,0.));
#4160=CARTESIAN_POINT('Origin',(0.,0.,0.));
#4161=CARTESIAN_POINT('',(-8.,-9.79717439317883E-16,0.));
#4162=CARTESIAN_POINT('Origin',(0.,0.,0.));
#4163=CARTESIAN_POINT('Origin',(0.,0.,-2.));
#4164=CARTESIAN_POINT('',(-8.,-9.79717439317883E-16,-2.));
#4165=CARTESIAN_POINT('',(-8.,-9.79717439317883E-16,-2.));
#4166=CARTESIAN_POINT('Origin',(0.,0.,-2.));
#4167=CARTESIAN_POINT('Origin',(0.,0.,-2.));
#4168=CARTESIAN_POINT('Origin',(0.,0.,0.));
#4169=CARTESIAN_POINT('',(-5.,-6.12323399573677E-16,0.));
#4170=CARTESIAN_POINT('Origin',(0.,0.,33.));
#4171=CARTESIAN_POINT('',(0.,0.,0.));
#4172=CARTESIAN_POINT('Origin',(0.,0.,23.));
#4173=CARTESIAN_POINT('',(-4.,-4.89858719658941E-16,22.));
#4174=CARTESIAN_POINT('Origin',(0.,0.,22.));
#4175=CARTESIAN_POINT('',(-4.,-4.89858719658941E-16,24.));
#4176=CARTESIAN_POINT('',(-4.,-4.89858719658941E-16,23.));
#4177=CARTESIAN_POINT('Origin',(0.,0.,24.));
#4178=CARTESIAN_POINT('Origin',(8.,0.,22.));
#4179=CARTESIAN_POINT('',(-5.,6.12323399573677E-16,22.));
#4180=CARTESIAN_POINT('Origin',(0.,0.,22.));
#4181=CARTESIAN_POINT('Origin',(4.,0.,24.));
#4182=CARTESIAN_POINT('',(-5.,-6.12323399573677E-16,24.));
#4183=CARTESIAN_POINT('Origin',(0.,0.,24.));
#4184=CARTESIAN_POINT('Origin',(0.,0.,0.));
#4185=CARTESIAN_POINT('',(-5.,-6.12323399573677E-16,25.));
#4186=CARTESIAN_POINT('Origin',(0.,0.,25.));
#4187=CARTESIAN_POINT('',(-5.,-6.12323399573677E-16,0.));
#4188=CARTESIAN_POINT('Origin',(0.,0.,0.));
#4189=CARTESIAN_POINT('',(-8.,-9.79717439317883E-16,0.));
#4190=CARTESIAN_POINT('Origin',(0.,0.,0.));
#4191=CARTESIAN_POINT('',(-5.,-6.12323399573677E-16,0.));
#4192=CARTESIAN_POINT('Origin',(0.,0.,0.));
#4193=CARTESIAN_POINT('Origin',(0.,0.,-2.));
#4194=CARTESIAN_POINT('',(-8.,-9.79717439317883E-16,-2.));
#4195=CARTESIAN_POINT('',(-8.,-9.79717439317883E-16,-2.));
#4196=CARTESIAN_POINT('Origin',(0.,0.,-2.));
#4197=CARTESIAN_POINT('Origin',(0.,0.,-2.));
#4198=CARTESIAN_POINT('Origin',(0.,0.,0.));
#4199=CARTESIAN_POINT('',(-5.,-6.12323399573677E-16,0.));
#4200=CARTESIAN_POINT('Origin',(0.,0.,25.));
#4201=CARTESIAN_POINT('',(0.,0.,0.));
#4202=CARTESIAN_POINT('Origin',(0.,0.,41.));
#4203=CARTESIAN_POINT('',(-4.,-4.89858719658941E-16,40.));
#4204=CARTESIAN_POINT('Origin',(0.,0.,40.));
#4205=CARTESIAN_POINT('',(-4.,-4.89858719658941E-16,42.));
#4206=CARTESIAN_POINT('',(-4.,-4.89858719658941E-16,41.));
#4207=CARTESIAN_POINT('Origin',(0.,0.,42.));
#4208=CARTESIAN_POINT('Origin',(8.,0.,40.));
#4209=CARTESIAN_POINT('',(-5.,6.12323399573677E-16,40.));
#4210=CARTESIAN_POINT('Origin',(0.,0.,40.));
#4211=CARTESIAN_POINT('Origin',(4.,0.,42.));
#4212=CARTESIAN_POINT('',(-5.,-6.12323399573677E-16,42.));
#4213=CARTESIAN_POINT('Origin',(0.,0.,42.));
#4214=CARTESIAN_POINT('Origin',(0.,0.,0.));
#4215=CARTESIAN_POINT('',(-5.,-6.12323399573677E-16,43.));
#4216=CARTESIAN_POINT('Origin',(0.,0.,43.));
#4217=CARTESIAN_POINT('',(-5.,-6.12323399573677E-16,0.));
#4218=CARTESIAN_POINT('Origin',(0.,0.,0.));
#4219=CARTESIAN_POINT('',(-8.,-9.79717439317883E-16,0.));
#4220=CARTESIAN_POINT('Origin',(0.,0.,0.));
#4221=CARTESIAN_POINT('',(-5.,-6.12323399573677E-16,0.));
#4222=CARTESIAN_POINT('Origin',(0.,0.,0.));
#4223=CARTESIAN_POINT('Origin',(0.,0.,-4.));
#4224=CARTESIAN_POINT('',(-8.,-9.79717439317883E-16,-4.));
#4225=CARTESIAN_POINT('',(-8.,-9.79717439317883E-16,-4.));
#4226=CARTESIAN_POINT('Origin',(0.,0.,-4.));
#4227=CARTESIAN_POINT('Origin',(0.,0.,-4.));
#4228=CARTESIAN_POINT('Origin',(0.,0.,0.));
#4229=CARTESIAN_POINT('',(-5.,-6.12323399573677E-16,0.));
#4230=CARTESIAN_POINT('Origin',(0.,0.,43.));
#4231=CARTESIAN_POINT('',(0.,0.,0.));
#4232=CARTESIAN_POINT('Origin',(0.,0.,0.));
#4233=CARTESIAN_POINT('',(-5.,-6.12323399573677E-16,8.));
#4234=CARTESIAN_POINT('Origin',(0.,0.,8.));
#4235=CARTESIAN_POINT('',(-5.,-6.12323399573677E-16,0.));
#4236=CARTESIAN_POINT('',(-5.,-6.12323399573677E-16,0.));
#4237=CARTESIAN_POINT('Origin',(0.,0.,0.));
#4238=CARTESIAN_POINT('Origin',(0.,0.,0.));
#4239=CARTESIAN_POINT('',(-7.,-8.57252759403147E-16,8.));
#4240=CARTESIAN_POINT('Origin',(0.,0.,8.));
#4241=CARTESIAN_POINT('',(-7.,-8.57252759403147E-16,0.));
#4242=CARTESIAN_POINT('',(-7.,-8.57252759403147E-16,0.));
#4243=CARTESIAN_POINT('Origin',(0.,0.,0.));
#4244=CARTESIAN_POINT('Origin',(0.,0.,8.));
#4245=CARTESIAN_POINT('Origin',(0.,0.,0.));
#4246=CARTESIAN_POINT('',(0.,0.,0.));
#4247=CARTESIAN_POINT('Origin',(0.,0.,0.));
#4248=CARTESIAN_POINT('',(-5.,-6.12323399573677E-16,10.));
#4249=CARTESIAN_POINT('Origin',(0.,0.,10.));
#4250=CARTESIAN_POINT('',(-5.,-6.12323399573677E-16,0.));
#4251=CARTESIAN_POINT('',(-5.,-6.12323399573677E-16,0.));
#4252=CARTESIAN_POINT('Origin',(0.,0.,0.));
#4253=CARTESIAN_POINT('Origin',(0.,0.,0.));
#4254=CARTESIAN_POINT('',(-7.,-8.57252759403147E-16,10.));
#4255=CARTESIAN_POINT('Origin',(0.,0.,10.));
#4256=CARTESIAN_POINT('',(-7.,-8.57252759403147E-16,0.));
#4257=CARTESIAN_POINT('',(-7.,-8.57252759403147E-16,0.));
#4258=CARTESIAN_POINT('Origin',(0.,0.,0.));
#4259=CARTESIAN_POINT('Origin',(0.,0.,10.));
#4260=CARTESIAN_POINT('Origin',(0.,0.,0.));
#4261=CARTESIAN_POINT('',(0.,0.,0.));
#4262=CARTESIAN_POINT('Origin',(0.,0.,0.));
#4263=CARTESIAN_POINT('',(-5.,-6.12323399573677E-16,2.));
#4264=CARTESIAN_POINT('Origin',(0.,0.,2.));
#4265=CARTESIAN_POINT('',(-5.,-6.12323399573677E-16,0.));
#4266=CARTESIAN_POINT('',(-5.,-6.12323399573677E-16,0.));
#4267=CARTESIAN_POINT('Origin',(0.,0.,0.));
#4268=CARTESIAN_POINT('Origin',(0.,0.,0.));
#4269=CARTESIAN_POINT('',(-10.,-1.22464679914735E-15,2.));
#4270=CARTESIAN_POINT('Origin',(0.,0.,2.));
#4271=CARTESIAN_POINT('',(-10.,-1.22464679914735E-15,0.));
#4272=CARTESIAN_POINT('',(-10.,-1.22464679914735E-15,0.));
#4273=CARTESIAN_POINT('Origin',(0.,0.,0.));
#4274=CARTESIAN_POINT('Origin',(0.,0.,2.));
#4275=CARTESIAN_POINT('Origin',(0.,0.,0.));
#4276=CARTESIAN_POINT('',(0.,0.,0.));
#4277=CARTESIAN_POINT('Origin',(-1.,0.,1.));
#4278=CARTESIAN_POINT('',(-1.,3.87298334620742,0.));
#4279=CARTESIAN_POINT('',(-1.,3.87298334620742,1.));
#4280=CARTESIAN_POINT('',(-1.,3.87298334620742,0.));
#4281=CARTESIAN_POINT('',(-1.,7.93725393319377,0.));
#4282=CARTESIAN_POINT('',(-1.,0.,0.));
#4283=CARTESIAN_POINT('',(-1.,7.93725393319377,1.));
#4284=CARTESIAN_POINT('',(-1.,7.93725393319377,0.));
#4285=CARTESIAN_POINT('',(-1.,0.,1.));
#4286=CARTESIAN_POINT('Origin',(1.,16.,1.));
#4287=CARTESIAN_POINT('',(1.,3.87298334620742,1.));
#4288=CARTESIAN_POINT('',(1.,3.87298334620742,0.));
#4289=CARTESIAN_POINT('',(1.,3.87298334620742,0.));
#4290=CARTESIAN_POINT('',(1.,7.93725393319377,1.));
#4291=CARTESIAN_POINT('',(1.,8.,1.));
#4292=CARTESIAN_POINT('',(1.,7.93725393319377,0.));
#4293=CARTESIAN_POINT('',(1.,7.93725393319377,0.));
#4294=CARTESIAN_POINT('',(1.,8.,0.));
#4295=CARTESIAN_POINT('Origin',(0.,0.,0.));
#4296=CARTESIAN_POINT('Origin',(0.,0.,0.));
#4297=CARTESIAN_POINT('Origin',(0.,0.,0.));
#4298=CARTESIAN_POINT('Origin',(0.,0.,0.));
#4299=CARTESIAN_POINT('Origin',(0.,0.,1.));
#4300=CARTESIAN_POINT('Origin',(0.,0.,0.));
#4301=CARTESIAN_POINT('Origin',(0.,0.,1.));
#4302=CARTESIAN_POINT('Origin',(0.,0.,1.));
#4303=CARTESIAN_POINT('',(0.,0.,0.));
#4304=CARTESIAN_POINT('',(80.,0.,10.));
#4305=CARTESIAN_POINT('',(0.,0.,10.));
#4306=CARTESIAN_POINT('',(80.,0.,20.));
#4307=CARTESIAN_POINT('',(-6.10249456578932E-16,1.93400440591702E-18,36.));
#4308=CARTESIAN_POINT('',(178.977722283739,-19.1565896266847,46.));
#4309=CARTESIAN_POINT('',(117.955308810476,-12.6251547753463,36.));
#4310=CARTESIAN_POINT('',(200.,139.456347549388,16.));
#4311=CARTESIAN_POINT('',(200.,139.456347549388,32.));
#4312=CARTESIAN_POINT('',(180.,-120.,10.));
#4313=CARTESIAN_POINT('',(180.,-130.,24.));
#4314=CARTESIAN_POINT('',(80.,0.,20.));
#4315=CARTESIAN_POINT('',(220.,-120.,10.));
#4316=CARTESIAN_POINT('',(180.,290.,10.));
#4317=CARTESIAN_POINT('',(220.,290.,10.));
#4318=CARTESIAN_POINT('',(220.,-130.,24.));
#4319=CARTESIAN_POINT('',(-6.10249456578932E-16,1.93400440591702E-18,36.));
#4320=CARTESIAN_POINT('',(80.,0.,0.));
#4321=CARTESIAN_POINT('',(0.,0.,0.));
#4322=CARTESIAN_POINT('',(117.955308810475,-12.6251547753464,18.));
#4323=CARTESIAN_POINT('',(178.977722283739,-19.1565896266847,34.));
#4324=CARTESIAN_POINT('',(200.,139.456347549388,16.));
#4325=CARTESIAN_POINT('',(80.,0.,28.));
#4326=CARTESIAN_POINT('',(117.955308810475,-12.6251547753464,20.));
#4327=CARTESIAN_POINT('',(178.977722283739,-19.1565896266847,46.));
#4328=CARTESIAN_POINT('',(200.,139.456347549387,46.));
#4329=CARTESIAN_POINT('',(178.977722283739,-19.1565896266846,36.));
#4330=CARTESIAN_POINT('',(80.,0.,31.));
#4331=CARTESIAN_POINT('',(0.,0.,46.));
#4332=CARTESIAN_POINT('',(117.955308810475,-12.6251547753464,18.));
#4333=CARTESIAN_POINT('',(117.955308810475,-12.6251547753464,46.));
#4334=CARTESIAN_POINT('',(178.977722283739,-19.1565896266847,34.));
#4335=CARTESIAN_POINT('',(178.977722283739,-19.1565896266847,54.0000000000001));
#4336=CARTESIAN_POINT('',(200.,139.456347549388,54.));
#4337=CARTESIAN_POINT('',(180.,300.,24.));
#4338=CARTESIAN_POINT('',(220.,300.,24.));
#4339=CARTESIAN_POINT('',(0.,0.,49.));
#4340=CARTESIAN_POINT('',(117.955308810475,-12.6251547753464,49.));
#4341=CARTESIAN_POINT('',(178.977722283739,-19.1565896266847,57.0000000000001));
#4342=CARTESIAN_POINT('',(200.,139.456347549388,57.));
#4343=CARTESIAN_POINT('',(180.,303.,24.));
#4344=CARTESIAN_POINT('',(220.,303.,24.));
#4345=UNCERTAINTY_MEASURE_WITH_UNIT(LENGTH_MEASURE(0.01),#4389,
'DISTANCE_ACCURACY_VALUE',
'Maximum model space distance between geometric entities at asserted c
onnectivities');
#4346=UNCERTAINTY_MEASURE_WITH_UNIT(LENGTH_MEASURE(0.01),#4389,
'DISTANCE_ACCURACY_VALUE',
'Maximum model space distance between geometric entities at asserted c
onnectivities');
#4347=UNCERTAINTY_MEASURE_WITH_UNIT(LENGTH_MEASURE(0.01),#4389,
'DISTANCE_ACCURACY_VALUE',
'Maximum model space distance between geometric entities at asserted c
onnectivities');
#4348=UNCERTAINTY_MEASURE_WITH_UNIT(LENGTH_MEASURE(0.01),#4389,
'DISTANCE_ACCURACY_VALUE',
'Maximum model space distance between geometric entities at asserted c
onnectivities');
#4349=UNCERTAINTY_MEASURE_WITH_UNIT(LENGTH_MEASURE(0.01),#4389,
'DISTANCE_ACCURACY_VALUE',
'Maximum model space distance between geometric entities at asserted c
onnectivities');
#4350=UNCERTAINTY_MEASURE_WITH_UNIT(LENGTH_MEASURE(0.01),#4389,
'DISTANCE_ACCURACY_VALUE',
'Maximum model space distance between geometric entities at asserted c
onnectivities');
#4351=UNCERTAINTY_MEASURE_WITH_UNIT(LENGTH_MEASURE(0.01),#4389,
'DISTANCE_ACCURACY_VALUE',
'Maximum model space distance between geometric entities at asserted c
onnectivities');
#4352=UNCERTAINTY_MEASURE_WITH_UNIT(LENGTH_MEASURE(0.01),#4389,
'DISTANCE_ACCURACY_VALUE',
'Maximum model space distance between geometric entities at asserted c
onnectivities');
#4353=UNCERTAINTY_MEASURE_WITH_UNIT(LENGTH_MEASURE(0.01),#4389,
'DISTANCE_ACCURACY_VALUE',
'Maximum model space distance between geometric entities at asserted c
onnectivities');
#4354=UNCERTAINTY_MEASURE_WITH_UNIT(LENGTH_MEASURE(0.01),#4389,
'DISTANCE_ACCURACY_VALUE',
'Maximum model space distance between geometric entities at asserted c
onnectivities');
#4355=UNCERTAINTY_MEASURE_WITH_UNIT(LENGTH_MEASURE(0.01),#4389,
'DISTANCE_ACCURACY_VALUE',
'Maximum model space distance between geometric entities at asserted c
onnectivities');
#4356=UNCERTAINTY_MEASURE_WITH_UNIT(LENGTH_MEASURE(0.01),#4389,
'DISTANCE_ACCURACY_VALUE',
'Maximum model space distance between geometric entities at asserted c
onnectivities');
#4357=UNCERTAINTY_MEASURE_WITH_UNIT(LENGTH_MEASURE(0.01),#4389,
'DISTANCE_ACCURACY_VALUE',
'Maximum model space distance between geometric entities at asserted c
onnectivities');
#4358=UNCERTAINTY_MEASURE_WITH_UNIT(LENGTH_MEASURE(0.01),#4389,
'DISTANCE_ACCURACY_VALUE',
'Maximum model space distance between geometric entities at asserted c
onnectivities');
#4359=UNCERTAINTY_MEASURE_WITH_UNIT(LENGTH_MEASURE(0.01),#4389,
'DISTANCE_ACCURACY_VALUE',
'Maximum model space distance between geometric entities at asserted c
onnectivities');
#4360=UNCERTAINTY_MEASURE_WITH_UNIT(LENGTH_MEASURE(0.01),#4389,
'DISTANCE_ACCURACY_VALUE',
'Maximum model space distance between geometric entities at asserted c
onnectivities');
#4361=UNCERTAINTY_MEASURE_WITH_UNIT(LENGTH_MEASURE(0.01),#4389,
'DISTANCE_ACCURACY_VALUE',
'Maximum model space distance between geometric entities at asserted c
onnectivities');
#4362=UNCERTAINTY_MEASURE_WITH_UNIT(LENGTH_MEASURE(0.01),#4389,
'DISTANCE_ACCURACY_VALUE',
'Maximum model space distance between geometric entities at asserted c
onnectivities');
#4363=UNCERTAINTY_MEASURE_WITH_UNIT(LENGTH_MEASURE(0.01),#4389,
'DISTANCE_ACCURACY_VALUE',
'Maximum model space distance between geometric entities at asserted c
onnectivities');
#4364=UNCERTAINTY_MEASURE_WITH_UNIT(LENGTH_MEASURE(0.01),#4389,
'DISTANCE_ACCURACY_VALUE',
'Maximum model space distance between geometric entities at asserted c
onnectivities');
#4365=UNCERTAINTY_MEASURE_WITH_UNIT(LENGTH_MEASURE(0.01),#4389,
'DISTANCE_ACCURACY_VALUE',
'Maximum model space distance between geometric entities at asserted c
onnectivities');
#4366=UNCERTAINTY_MEASURE_WITH_UNIT(LENGTH_MEASURE(0.01),#4389,
'DISTANCE_ACCURACY_VALUE',
'Maximum model space distance between geometric entities at asserted c
onnectivities');
#4367=(
GEOMETRIC_REPRESENTATION_CONTEXT(3)
GLOBAL_UNCERTAINTY_ASSIGNED_CONTEXT((#4345))
GLOBAL_UNIT_ASSIGNED_CONTEXT((#4389,#4391,#4392))
REPRESENTATION_CONTEXT('','3D')
);
#4368=(
GEOMETRIC_REPRESENTATION_CONTEXT(3)
GLOBAL_UNCERTAINTY_ASSIGNED_CONTEXT((#4346))
GLOBAL_UNIT_ASSIGNED_CONTEXT((#4389,#4391,#4392))
REPRESENTATION_CONTEXT('','3D')
);
#4369=(
GEOMETRIC_REPRESENTATION_CONTEXT(3)
GLOBAL_UNCERTAINTY_ASSIGNED_CONTEXT((#4347))
GLOBAL_UNIT_ASSIGNED_CONTEXT((#4389,#4391,#4392))
REPRESENTATION_CONTEXT('','3D')
);
#4370=(
GEOMETRIC_REPRESENTATION_CONTEXT(3)
GLOBAL_UNCERTAINTY_ASSIGNED_CONTEXT((#4348))
GLOBAL_UNIT_ASSIGNED_CONTEXT((#4389,#4391,#4392))
REPRESENTATION_CONTEXT('','3D')
);
#4371=(
GEOMETRIC_REPRESENTATION_CONTEXT(3)
GLOBAL_UNCERTAINTY_ASSIGNED_CONTEXT((#4349))
GLOBAL_UNIT_ASSIGNED_CONTEXT((#4389,#4391,#4392))
REPRESENTATION_CONTEXT('','3D')
);
#4372=(
GEOMETRIC_REPRESENTATION_CONTEXT(3)
GLOBAL_UNCERTAINTY_ASSIGNED_CONTEXT((#4350))
GLOBAL_UNIT_ASSIGNED_CONTEXT((#4389,#4391,#4392))
REPRESENTATION_CONTEXT('','3D')
);
#4373=(
GEOMETRIC_REPRESENTATION_CONTEXT(3)
GLOBAL_UNCERTAINTY_ASSIGNED_CONTEXT((#4351))
GLOBAL_UNIT_ASSIGNED_CONTEXT((#4389,#4391,#4392))
REPRESENTATION_CONTEXT('','3D')
);
#4374=(
GEOMETRIC_REPRESENTATION_CONTEXT(3)
GLOBAL_UNCERTAINTY_ASSIGNED_CONTEXT((#4352))
GLOBAL_UNIT_ASSIGNED_CONTEXT((#4389,#4391,#4392))
REPRESENTATION_CONTEXT('','3D')
);
#4375=(
GEOMETRIC_REPRESENTATION_CONTEXT(3)
GLOBAL_UNCERTAINTY_ASSIGNED_CONTEXT((#4353))
GLOBAL_UNIT_ASSIGNED_CONTEXT((#4389,#4391,#4392))
REPRESENTATION_CONTEXT('','3D')
);
#4376=(
GEOMETRIC_REPRESENTATION_CONTEXT(3)
GLOBAL_UNCERTAINTY_ASSIGNED_CONTEXT((#4354))
GLOBAL_UNIT_ASSIGNED_CONTEXT((#4389,#4391,#4392))
REPRESENTATION_CONTEXT('','3D')
);
#4377=(
GEOMETRIC_REPRESENTATION_CONTEXT(3)
GLOBAL_UNCERTAINTY_ASSIGNED_CONTEXT((#4355))
GLOBAL_UNIT_ASSIGNED_CONTEXT((#4389,#4391,#4392))
REPRESENTATION_CONTEXT('','3D')
);
#4378=(
GEOMETRIC_REPRESENTATION_CONTEXT(3)
GLOBAL_UNCERTAINTY_ASSIGNED_CONTEXT((#4356))
GLOBAL_UNIT_ASSIGNED_CONTEXT((#4389,#4391,#4392))
REPRESENTATION_CONTEXT('','3D')
);
#4379=(
GEOMETRIC_REPRESENTATION_CONTEXT(3)
GLOBAL_UNCERTAINTY_ASSIGNED_CONTEXT((#4357))
GLOBAL_UNIT_ASSIGNED_CONTEXT((#4389,#4391,#4392))
REPRESENTATION_CONTEXT('','3D')
);
#4380=(
GEOMETRIC_REPRESENTATION_CONTEXT(3)
GLOBAL_UNCERTAINTY_ASSIGNED_CONTEXT((#4358))
GLOBAL_UNIT_ASSIGNED_CONTEXT((#4389,#4391,#4392))
REPRESENTATION_CONTEXT('','3D')
);
#4381=(
GEOMETRIC_REPRESENTATION_CONTEXT(3)
GLOBAL_UNCERTAINTY_ASSIGNED_CONTEXT((#4359))
GLOBAL_UNIT_ASSIGNED_CONTEXT((#4389,#4391,#4392))
REPRESENTATION_CONTEXT('','3D')
);
#4382=(
GEOMETRIC_REPRESENTATION_CONTEXT(3)
GLOBAL_UNCERTAINTY_ASSIGNED_CONTEXT((#4360))
GLOBAL_UNIT_ASSIGNED_CONTEXT((#4389,#4391,#4392))
REPRESENTATION_CONTEXT('','3D')
);
#4383=(
GEOMETRIC_REPRESENTATION_CONTEXT(3)
GLOBAL_UNCERTAINTY_ASSIGNED_CONTEXT((#4361))
GLOBAL_UNIT_ASSIGNED_CONTEXT((#4389,#4391,#4392))
REPRESENTATION_CONTEXT('','3D')
);
#4384=(
GEOMETRIC_REPRESENTATION_CONTEXT(3)
GLOBAL_UNCERTAINTY_ASSIGNED_CONTEXT((#4362))
GLOBAL_UNIT_ASSIGNED_CONTEXT((#4389,#4391,#4392))
REPRESENTATION_CONTEXT('','3D')
);
#4385=(
GEOMETRIC_REPRESENTATION_CONTEXT(3)
GLOBAL_UNCERTAINTY_ASSIGNED_CONTEXT((#4363))
GLOBAL_UNIT_ASSIGNED_CONTEXT((#4389,#4391,#4392))
REPRESENTATION_CONTEXT('','3D')
);
#4386=(
GEOMETRIC_REPRESENTATION_CONTEXT(3)
GLOBAL_UNCERTAINTY_ASSIGNED_CONTEXT((#4364))
GLOBAL_UNIT_ASSIGNED_CONTEXT((#4389,#4391,#4392))
REPRESENTATION_CONTEXT('','3D')
);
#4387=(
GEOMETRIC_REPRESENTATION_CONTEXT(3)
GLOBAL_UNCERTAINTY_ASSIGNED_CONTEXT((#4365))
GLOBAL_UNIT_ASSIGNED_CONTEXT((#4389,#4391,#4392))
REPRESENTATION_CONTEXT('','3D')
);
#4388=(
GEOMETRIC_REPRESENTATION_CONTEXT(3)
GLOBAL_UNCERTAINTY_ASSIGNED_CONTEXT((#4366))
GLOBAL_UNIT_ASSIGNED_CONTEXT((#4389,#4391,#4392))
REPRESENTATION_CONTEXT('','3D')
);
#4389=(
LENGTH_UNIT()
NAMED_UNIT(*)
SI_UNIT(.MILLI.,.METRE.)
);
#4390=(
LENGTH_UNIT()
NAMED_UNIT(*)
SI_UNIT($,.METRE.)
);
#4391=(
NAMED_UNIT(*)
PLANE_ANGLE_UNIT()
SI_UNIT($,.RADIAN.)
);
#4392=(
NAMED_UNIT(*)
SI_UNIT($,.STERADIAN.)
SOLID_ANGLE_UNIT()
);
#4393=SHAPE_DEFINITION_REPRESENTATION(#4414,#4477);
#4394=SHAPE_DEFINITION_REPRESENTATION(#4415,#4478);
#4395=SHAPE_DEFINITION_REPRESENTATION(#4416,#4479);
#4396=SHAPE_DEFINITION_REPRESENTATION(#4417,#4480);
#4397=SHAPE_DEFINITION_REPRESENTATION(#4418,#4481);
#4398=SHAPE_DEFINITION_REPRESENTATION(#4419,#4482);
#4399=SHAPE_DEFINITION_REPRESENTATION(#4420,#4483);
#4400=SHAPE_DEFINITION_REPRESENTATION(#4421,#4484);
#4401=SHAPE_DEFINITION_REPRESENTATION(#4422,#4485);
#4402=SHAPE_DEFINITION_REPRESENTATION(#4423,#4486);
#4403=SHAPE_DEFINITION_REPRESENTATION(#4424,#4487);
#4404=SHAPE_DEFINITION_REPRESENTATION(#4425,#4488);
#4405=SHAPE_DEFINITION_REPRESENTATION(#4426,#4489);
#4406=SHAPE_DEFINITION_REPRESENTATION(#4427,#4490);
#4407=SHAPE_DEFINITION_REPRESENTATION(#4428,#4491);
#4408=SHAPE_DEFINITION_REPRESENTATION(#4429,#4492);
#4409=SHAPE_DEFINITION_REPRESENTATION(#4430,#4493);
#4410=SHAPE_DEFINITION_REPRESENTATION(#4431,#4494);
#4411=SHAPE_DEFINITION_REPRESENTATION(#4432,#4495);
#4412=SHAPE_DEFINITION_REPRESENTATION(#4433,#4496);
#4413=SHAPE_DEFINITION_REPRESENTATION(#4434,#4497);
#4414=PRODUCT_DEFINITION_SHAPE('',$,#4499);
#4415=PRODUCT_DEFINITION_SHAPE('',$,#4500);
#4416=PRODUCT_DEFINITION_SHAPE('',$,#4501);
#4417=PRODUCT_DEFINITION_SHAPE('',$,#4502);
#4418=PRODUCT_DEFINITION_SHAPE('',$,#4503);
#4419=PRODUCT_DEFINITION_SHAPE('',$,#4504);
#4420=PRODUCT_DEFINITION_SHAPE('',$,#4505);
#4421=PRODUCT_DEFINITION_SHAPE('',$,#4506);
#4422=PRODUCT_DEFINITION_SHAPE('',$,#4507);
#4423=PRODUCT_DEFINITION_SHAPE('',$,#4508);
#4424=PRODUCT_DEFINITION_SHAPE('',$,#4509);
#4425=PRODUCT_DEFINITION_SHAPE('',$,#4510);
#4426=PRODUCT_DEFINITION_SHAPE('',$,#4511);
#4427=PRODUCT_DEFINITION_SHAPE('',$,#4512);
#4428=PRODUCT_DEFINITION_SHAPE('',$,#4513);
#4429=PRODUCT_DEFINITION_SHAPE('',$,#4514);
#4430=PRODUCT_DEFINITION_SHAPE('',$,#4515);
#4431=PRODUCT_DEFINITION_SHAPE('',$,#4516);
#4432=PRODUCT_DEFINITION_SHAPE('',$,#4517);
#4433=PRODUCT_DEFINITION_SHAPE('',$,#4518);
#4434=PRODUCT_DEFINITION_SHAPE('',$,#4519);
#4435=PRODUCT_DEFINITION_SHAPE($,$,#137);
#4436=PRODUCT_DEFINITION_SHAPE($,$,#138);
#4437=PRODUCT_DEFINITION_SHAPE($,$,#139);
#4438=PRODUCT_DEFINITION_SHAPE($,$,#140);
#4439=PRODUCT_DEFINITION_SHAPE($,$,#141);
#4440=PRODUCT_DEFINITION_SHAPE($,$,#142);
#4441=PRODUCT_DEFINITION_SHAPE($,$,#143);
#4442=PRODUCT_DEFINITION_SHAPE($,$,#144);
#4443=PRODUCT_DEFINITION_SHAPE($,$,#145);
#4444=PRODUCT_DEFINITION_SHAPE($,$,#146);
#4445=PRODUCT_DEFINITION_SHAPE($,$,#147);
#4446=PRODUCT_DEFINITION_SHAPE($,$,#148);
#4447=PRODUCT_DEFINITION_SHAPE($,$,#149);
#4448=PRODUCT_DEFINITION_SHAPE($,$,#150);
#4449=PRODUCT_DEFINITION_SHAPE($,$,#151);
#4450=PRODUCT_DEFINITION_SHAPE($,$,#152);
#4451=PRODUCT_DEFINITION_SHAPE($,$,#153);
#4452=PRODUCT_DEFINITION_SHAPE($,$,#154);
#4453=PRODUCT_DEFINITION_SHAPE($,$,#155);
#4454=PRODUCT_DEFINITION_SHAPE($,$,#156);
#4455=PRODUCT_DEFINITION_SHAPE($,$,#157);
#4456=PRODUCT_DEFINITION_SHAPE($,$,#158);
#4457=PRODUCT_DEFINITION_SHAPE($,$,#159);
#4458=PRODUCT_DEFINITION_SHAPE($,$,#160);
#4459=PRODUCT_DEFINITION_SHAPE($,$,#161);
#4460=PRODUCT_DEFINITION_SHAPE($,$,#162);
#4461=PRODUCT_DEFINITION_SHAPE($,$,#163);
#4462=PRODUCT_DEFINITION_SHAPE($,$,#164);
#4463=PRODUCT_DEFINITION_SHAPE($,$,#165);
#4464=PRODUCT_DEFINITION_SHAPE($,$,#166);
#4465=PRODUCT_DEFINITION_SHAPE($,$,#167);
#4466=PRODUCT_DEFINITION_SHAPE($,$,#168);
#4467=PRODUCT_DEFINITION_SHAPE($,$,#169);
#4468=PRODUCT_DEFINITION_SHAPE($,$,#170);
#4469=PRODUCT_DEFINITION_SHAPE($,$,#171);
#4470=PRODUCT_DEFINITION_SHAPE($,$,#172);
#4471=PRODUCT_DEFINITION_SHAPE($,$,#173);
#4472=PRODUCT_DEFINITION_SHAPE($,$,#174);
#4473=PRODUCT_DEFINITION_SHAPE($,$,#175);
#4474=PRODUCT_DEFINITION_SHAPE($,$,#176);
#4475=PRODUCT_DEFINITION_SHAPE($,$,#177);
#4476=PRODUCT_DEFINITION_SHAPE($,$,#178);
#4477=SHAPE_REPRESENTATION('',(#2565,#2855,#2856,#2857,#2858,#2859,#2860,
#2861,#2862,#2863,#2864,#2865,#2866,#2867,#2868,#2869,#2870,#2871,#2872,
#2873,#2874,#2875,#2876,#2877,#2878,#2879,#2880,#2881,#2882,#2883,#2884,
#2885,#2886,#2887,#2888,#2889,#2890,#2891,#2892,#2893,#2894,#2895,#2896),
#4367);
#4478=SHAPE_REPRESENTATION('',(#2566),#4368);
#4479=SHAPE_REPRESENTATION('',(#2579),#4369);
#4480=SHAPE_REPRESENTATION('',(#2588),#4370);
#4481=SHAPE_REPRESENTATION('',(#2597),#4371);
#4482=SHAPE_REPRESENTATION('',(#2614),#4372);
#4483=SHAPE_REPRESENTATION('',(#2639),#4373);
#4484=SHAPE_REPRESENTATION('',(#2656),#4374);
#4485=SHAPE_REPRESENTATION('',(#2666),#4375);
#4486=SHAPE_REPRESENTATION('',(#2682),#4376);
#4487=SHAPE_REPRESENTATION('',(#2691),#4377);
#4488=SHAPE_REPRESENTATION('',(#2701),#4378);
#4489=SHAPE_REPRESENTATION('',(#2719),#4379);
#4490=SHAPE_REPRESENTATION('',(#2737),#4380);
#4491=SHAPE_REPRESENTATION('',(#2755),#4381);
#4492=SHAPE_REPRESENTATION('',(#2781),#4382);
#4493=SHAPE_REPRESENTATION('',(#2799),#4383);
#4494=SHAPE_REPRESENTATION('',(#2817),#4384);
#4495=SHAPE_REPRESENTATION('',(#2826),#4385);
#4496=SHAPE_REPRESENTATION('',(#2835),#4386);
#4497=SHAPE_REPRESENTATION('',(#2844),#4387);
#4498=PRODUCT_DEFINITION_CONTEXT('part definition',#4563,'design');
#4499=PRODUCT_DEFINITION('MAS-235','MAS-235',#4520,#4498);
#4500=PRODUCT_DEFINITION('Base plate','Base plate',#4521,#4498);
#4501=PRODUCT_DEFINITION('Crank pedestal','Crank pedestal',#4522,#4498);
#4502=PRODUCT_DEFINITION('Lever pedestal','Lever pedestal',#4523,#4498);
#4503=PRODUCT_DEFINITION('Driving crank','Driving crank',#4524,#4498);
#4504=PRODUCT_DEFINITION('Slotted lever','Slotted lever',#4525,#4498);
#4505=PRODUCT_DEFINITION('Connecting rod','Connecting rod',#4526,#4498);
#4506=PRODUCT_DEFINITION('Sliding block','Sliding block',#4527,#4498);
#4507=PRODUCT_DEFINITION('Output carriage','Output carriage',#4528,#4498);
#4508=PRODUCT_DEFINITION('Output pivot boss','Output pivot boss',#4529,
#4498);
#4509=PRODUCT_DEFINITION('Guide support','Guide support',#4530,#4498);
#4510=PRODUCT_DEFINITION('Guide rod','Guide rod',#4531,#4498);
#4511=PRODUCT_DEFINITION('Crank ground pin','Crank ground pin',#4532,#4498);
#4512=PRODUCT_DEFINITION('Lever ground pin','Lever ground pin',#4533,#4498);
#4513=PRODUCT_DEFINITION('Crank pin','Crank pin',#4534,#4498);
#4514=PRODUCT_DEFINITION('Link pivot pin','Link pivot pin',#4535,#4498);
#4515=PRODUCT_DEFINITION('Output pivot pin','Output pivot pin',#4536,#4498);
#4516=PRODUCT_DEFINITION('Pivot bushing','Pivot bushing',#4537,#4498);
#4517=PRODUCT_DEFINITION('Lever bushing','Lever bushing',#4538,#4498);
#4518=PRODUCT_DEFINITION('Pivot washer','Pivot washer',#4539,#4498);
#4519=PRODUCT_DEFINITION('Pivot retaining ring','Pivot retaining ring',
#4540,#4498);
#4520=PRODUCT_DEFINITION_FORMATION('',$,#4565);
#4521=PRODUCT_DEFINITION_FORMATION('',$,#4566);
#4522=PRODUCT_DEFINITION_FORMATION('',$,#4567);
#4523=PRODUCT_DEFINITION_FORMATION('',$,#4568);
#4524=PRODUCT_DEFINITION_FORMATION('',$,#4569);
#4525=PRODUCT_DEFINITION_FORMATION('',$,#4570);
#4526=PRODUCT_DEFINITION_FORMATION('',$,#4571);
#4527=PRODUCT_DEFINITION_FORMATION('',$,#4572);
#4528=PRODUCT_DEFINITION_FORMATION('',$,#4573);
#4529=PRODUCT_DEFINITION_FORMATION('',$,#4574);
#4530=PRODUCT_DEFINITION_FORMATION('',$,#4575);
#4531=PRODUCT_DEFINITION_FORMATION('',$,#4576);
#4532=PRODUCT_DEFINITION_FORMATION('',$,#4577);
#4533=PRODUCT_DEFINITION_FORMATION('',$,#4578);
#4534=PRODUCT_DEFINITION_FORMATION('',$,#4579);
#4535=PRODUCT_DEFINITION_FORMATION('',$,#4580);
#4536=PRODUCT_DEFINITION_FORMATION('',$,#4581);
#4537=PRODUCT_DEFINITION_FORMATION('',$,#4582);
#4538=PRODUCT_DEFINITION_FORMATION('',$,#4583);
#4539=PRODUCT_DEFINITION_FORMATION('',$,#4584);
#4540=PRODUCT_DEFINITION_FORMATION('',$,#4585);
#4541=PRODUCT_RELATED_PRODUCT_CATEGORY('MAS-235','MAS-235',(#4565));
#4542=PRODUCT_RELATED_PRODUCT_CATEGORY('Base plate','Base plate',(#4566));
#4543=PRODUCT_RELATED_PRODUCT_CATEGORY('Crank pedestal',
'Crank pedestal',(#4567));
#4544=PRODUCT_RELATED_PRODUCT_CATEGORY('Lever pedestal',
'Lever pedestal',(#4568));
#4545=PRODUCT_RELATED_PRODUCT_CATEGORY('Driving crank','Driving crank',
(#4569));
#4546=PRODUCT_RELATED_PRODUCT_CATEGORY('Slotted lever','Slotted lever',
(#4570));
#4547=PRODUCT_RELATED_PRODUCT_CATEGORY('Connecting rod',
'Connecting rod',(#4571));
#4548=PRODUCT_RELATED_PRODUCT_CATEGORY('Sliding block','Sliding block',
(#4572));
#4549=PRODUCT_RELATED_PRODUCT_CATEGORY('Output carriage',
'Output carriage',(#4573));
#4550=PRODUCT_RELATED_PRODUCT_CATEGORY('Output pivot boss',
'Output pivot boss',(#4574));
#4551=PRODUCT_RELATED_PRODUCT_CATEGORY('Guide support','Guide support',
(#4575));
#4552=PRODUCT_RELATED_PRODUCT_CATEGORY('Guide rod','Guide rod',(#4576));
#4553=PRODUCT_RELATED_PRODUCT_CATEGORY('Crank ground pin',
'Crank ground pin',(#4577));
#4554=PRODUCT_RELATED_PRODUCT_CATEGORY('Lever ground pin',
'Lever ground pin',(#4578));
#4555=PRODUCT_RELATED_PRODUCT_CATEGORY('Crank pin','Crank pin',(#4579));
#4556=PRODUCT_RELATED_PRODUCT_CATEGORY('Link pivot pin',
'Link pivot pin',(#4580));
#4557=PRODUCT_RELATED_PRODUCT_CATEGORY('Output pivot pin',
'Output pivot pin',(#4581));
#4558=PRODUCT_RELATED_PRODUCT_CATEGORY('Pivot bushing','Pivot bushing',
(#4582));
#4559=PRODUCT_RELATED_PRODUCT_CATEGORY('Lever bushing','Lever bushing',
(#4583));
#4560=PRODUCT_RELATED_PRODUCT_CATEGORY('Pivot washer','Pivot washer',(#4584));
#4561=PRODUCT_RELATED_PRODUCT_CATEGORY('Pivot retaining ring',
'Pivot retaining ring',(#4585));
#4562=APPLICATION_PROTOCOL_DEFINITION('international standard',
'automotive_design',2009,#4563);
#4563=APPLICATION_CONTEXT(
'Core Data for Automotive Mechanical Design Process');
#4564=PRODUCT_CONTEXT('part definition',#4563,'mechanical');
#4565=PRODUCT('MAS-235','MAS-235',
'Independent Whitworth quick-return mechanism. Crank radius40, ground-
center spacing80, lever180, connecting rod160, output guide X200. Nomi
nal stroke180 and long/short phase ratio2. Retained guide rods, replac
eable bearing sleeves and captured sliding shoe. No load or production
 rating assigned.',(#4564));
#4566=PRODUCT('Base plate','Base plate','Base plate',(#4564));
#4567=PRODUCT('Crank pedestal','Crank pedestal',$,(#4564));
#4568=PRODUCT('Lever pedestal','Lever pedestal',$,(#4564));
#4569=PRODUCT('Driving crank','Driving crank','Driving crank',(#4564));
#4570=PRODUCT('Slotted lever','Slotted lever','Slotted lever',(#4564));
#4571=PRODUCT('Connecting rod','Connecting rod','Connecting rod',(#4564));
#4572=PRODUCT('Sliding block','Sliding block',$,(#4564));
#4573=PRODUCT('Output carriage','Output carriage',$,(#4564));
#4574=PRODUCT('Output pivot boss','Output pivot boss',$,(#4564));
#4575=PRODUCT('Guide support','Guide support',$,(#4564));
#4576=PRODUCT('Guide rod','Guide rod',$,(#4564));
#4577=PRODUCT('Crank ground pin','Crank ground pin',$,(#4564));
#4578=PRODUCT('Lever ground pin','Lever ground pin',$,(#4564));
#4579=PRODUCT('Crank pin','Crank pin','Crank pin',(#4564));
#4580=PRODUCT('Link pivot pin','Link pivot pin',$,(#4564));
#4581=PRODUCT('Output pivot pin','Output pivot pin',$,(#4564));
#4582=PRODUCT('Pivot bushing','Pivot bushing',$,(#4564));
#4583=PRODUCT('Lever bushing','Lever bushing',$,(#4564));
#4584=PRODUCT('Pivot washer','Pivot washer',$,(#4564));
#4585=PRODUCT('Pivot retaining ring','Pivot retaining ring',$,(#4564));
#4586=PRESENTATION_STYLE_ASSIGNMENT((#4600));
#4587=PRESENTATION_STYLE_ASSIGNMENT((#4601));
#4588=PRESENTATION_STYLE_ASSIGNMENT((#4602));
#4589=PRESENTATION_STYLE_ASSIGNMENT((#4603));
#4590=PRESENTATION_STYLE_ASSIGNMENT((#4604));
#4591=PRESENTATION_STYLE_ASSIGNMENT((#4605));
#4592=PRESENTATION_STYLE_ASSIGNMENT((#4606));
#4593=PRESENTATION_STYLE_ASSIGNMENT((#4607));
#4594=PRESENTATION_STYLE_ASSIGNMENT((#4608));
#4595=PRESENTATION_STYLE_ASSIGNMENT((#4609));
#4596=PRESENTATION_STYLE_ASSIGNMENT((#4610));
#4597=PRESENTATION_STYLE_ASSIGNMENT((#4611));
#4598=PRESENTATION_STYLE_ASSIGNMENT((#4612));
#4599=PRESENTATION_STYLE_ASSIGNMENT((#4613));
#4600=SURFACE_STYLE_USAGE(.BOTH.,#4614);
#4601=SURFACE_STYLE_USAGE(.BOTH.,#4615);
#4602=SURFACE_STYLE_USAGE(.BOTH.,#4616);
#4603=SURFACE_STYLE_USAGE(.BOTH.,#4617);
#4604=SURFACE_STYLE_USAGE(.BOTH.,#4618);
#4605=SURFACE_STYLE_USAGE(.BOTH.,#4619);
#4606=SURFACE_STYLE_USAGE(.BOTH.,#4620);
#4607=SURFACE_STYLE_USAGE(.BOTH.,#4621);
#4608=SURFACE_STYLE_USAGE(.BOTH.,#4622);
#4609=SURFACE_STYLE_USAGE(.BOTH.,#4623);
#4610=SURFACE_STYLE_USAGE(.BOTH.,#4624);
#4611=SURFACE_STYLE_USAGE(.BOTH.,#4625);
#4612=SURFACE_STYLE_USAGE(.BOTH.,#4626);
#4613=SURFACE_STYLE_USAGE(.BOTH.,#4627);
#4614=SURFACE_SIDE_STYLE('',(#4628));
#4615=SURFACE_SIDE_STYLE('',(#4629));
#4616=SURFACE_SIDE_STYLE('',(#4630));
#4617=SURFACE_SIDE_STYLE('',(#4631));
#4618=SURFACE_SIDE_STYLE('',(#4632));
#4619=SURFACE_SIDE_STYLE('',(#4633));
#4620=SURFACE_SIDE_STYLE('',(#4634));
#4621=SURFACE_SIDE_STYLE('',(#4635));
#4622=SURFACE_SIDE_STYLE('',(#4636));
#4623=SURFACE_SIDE_STYLE('',(#4637));
#4624=SURFACE_SIDE_STYLE('',(#4638));
#4625=SURFACE_SIDE_STYLE('',(#4639));
#4626=SURFACE_SIDE_STYLE('',(#4640));
#4627=SURFACE_SIDE_STYLE('',(#4641));
#4628=SURFACE_STYLE_FILL_AREA(#4642);
#4629=SURFACE_STYLE_FILL_AREA(#4643);
#4630=SURFACE_STYLE_FILL_AREA(#4644);
#4631=SURFACE_STYLE_FILL_AREA(#4645);
#4632=SURFACE_STYLE_FILL_AREA(#4646);
#4633=SURFACE_STYLE_FILL_AREA(#4647);
#4634=SURFACE_STYLE_FILL_AREA(#4648);
#4635=SURFACE_STYLE_FILL_AREA(#4649);
#4636=SURFACE_STYLE_FILL_AREA(#4650);
#4637=SURFACE_STYLE_FILL_AREA(#4651);
#4638=SURFACE_STYLE_FILL_AREA(#4652);
#4639=SURFACE_STYLE_FILL_AREA(#4653);
#4640=SURFACE_STYLE_FILL_AREA(#4654);
#4641=SURFACE_STYLE_FILL_AREA(#4655);
#4642=FILL_AREA_STYLE('Steel - Satin',(#4656));
#4643=FILL_AREA_STYLE('Base gray',(#4657));
#4644=FILL_AREA_STYLE('Support gray',(#4658));
#4645=FILL_AREA_STYLE('Driving crank finish',(#4659));
#4646=FILL_AREA_STYLE('Sky blue',(#4660));
#4647=FILL_AREA_STYLE('Connecting rod finish',(#4661));
#4648=FILL_AREA_STYLE('Shoe gray',(#4662));
#4649=FILL_AREA_STYLE('Dark blue',(#4663));
#4650=FILL_AREA_STYLE('Boss gray',(#4664));
#4651=FILL_AREA_STYLE('Pivot gray',(#4665));
#4652=FILL_AREA_STYLE('Bearing light gray',(#4666));
#4653=FILL_AREA_STYLE('Bearing gray',(#4667));
#4654=FILL_AREA_STYLE('Washer light gray',(#4668));
#4655=FILL_AREA_STYLE('Dark gray',(#4669));
#4656=FILL_AREA_STYLE_COLOUR('Steel - Satin',#4670);
#4657=FILL_AREA_STYLE_COLOUR('Base gray',#4671);
#4658=FILL_AREA_STYLE_COLOUR('Support gray',#4672);
#4659=FILL_AREA_STYLE_COLOUR('Driving crank finish',#4673);
#4660=FILL_AREA_STYLE_COLOUR('Sky blue',#4674);
#4661=FILL_AREA_STYLE_COLOUR('Connecting rod finish',#4675);
#4662=FILL_AREA_STYLE_COLOUR('Shoe gray',#4676);
#4663=FILL_AREA_STYLE_COLOUR('Dark blue',#4677);
#4664=FILL_AREA_STYLE_COLOUR('Boss gray',#4678);
#4665=FILL_AREA_STYLE_COLOUR('Pivot gray',#4679);
#4666=FILL_AREA_STYLE_COLOUR('Bearing light gray',#4680);
#4667=FILL_AREA_STYLE_COLOUR('Bearing gray',#4681);
#4668=FILL_AREA_STYLE_COLOUR('Washer light gray',#4682);
#4669=FILL_AREA_STYLE_COLOUR('Dark gray',#4683);
#4670=COLOUR_RGB('Steel - Satin',0.627450980392157,0.627450980392157,0.627450980392157);
#4671=COLOUR_RGB('Base gray',0.407843137254902,0.447058823529412,0.498039215686275);
#4672=COLOUR_RGB('Support gray',0.407843137254902,0.447058823529412,0.498039215686275);
#4673=COLOUR_RGB('Driving crank finish',0.0901960784313725,0.270588235294118,
0.513725490196078);
#4674=COLOUR_RGB('Sky blue',0.317647058823529,0.686274509803922,0.890196078431372);
#4675=COLOUR_RGB('Connecting rod finish',0.662745098039216,0.831372549019608,
0.949019607843137);
#4676=COLOUR_RGB('Shoe gray',0.407843137254902,0.447058823529412,0.498039215686275);
#4677=COLOUR_RGB('Dark blue',0.0901960784313725,0.270588235294118,0.513725490196078);
#4678=COLOUR_RGB('Boss gray',0.407843137254902,0.447058823529412,0.498039215686275);
#4679=COLOUR_RGB('Pivot gray',0.407843137254902,0.447058823529412,0.498039215686275);
#4680=COLOUR_RGB('Bearing light gray',0.725490196078431,0.752941176470588,
0.792156862745098);
#4681=COLOUR_RGB('Bearing gray',0.725490196078431,0.752941176470588,0.792156862745098);
#4682=COLOUR_RGB('Washer light gray',0.725490196078431,0.752941176470588,
0.792156862745098);
#4683=COLOUR_RGB('Dark gray',0.250980392156863,0.282352941176471,0.32156862745098);
ENDSEC;
END-ISO-10303-21;
